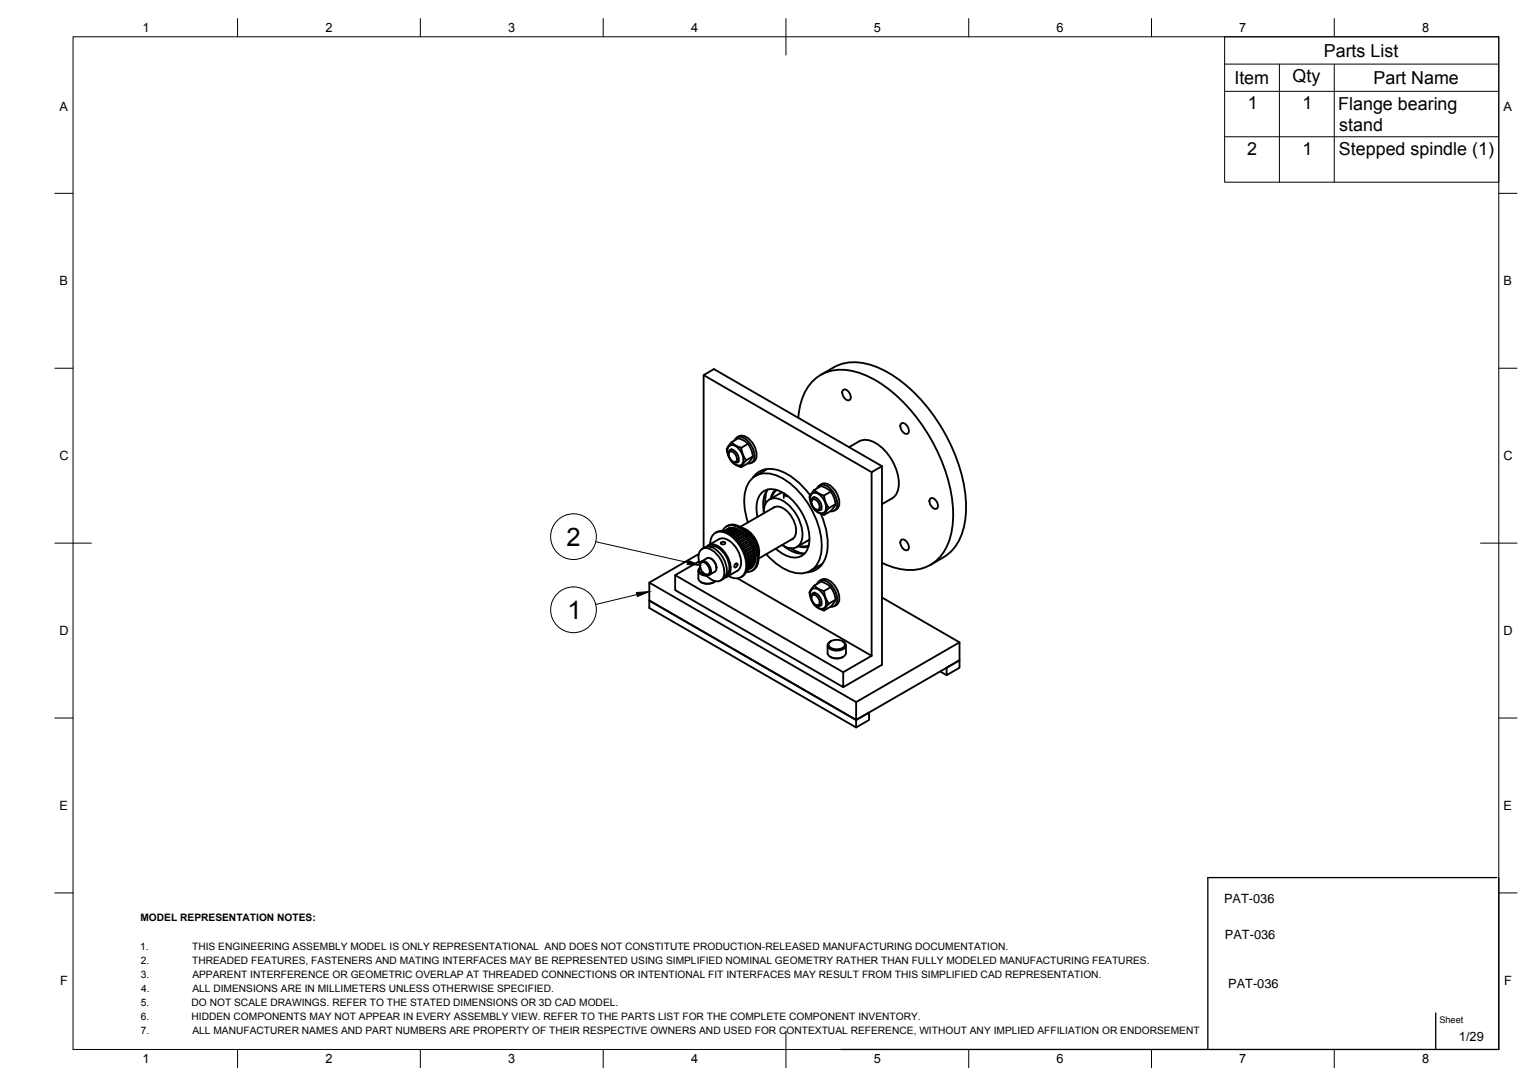
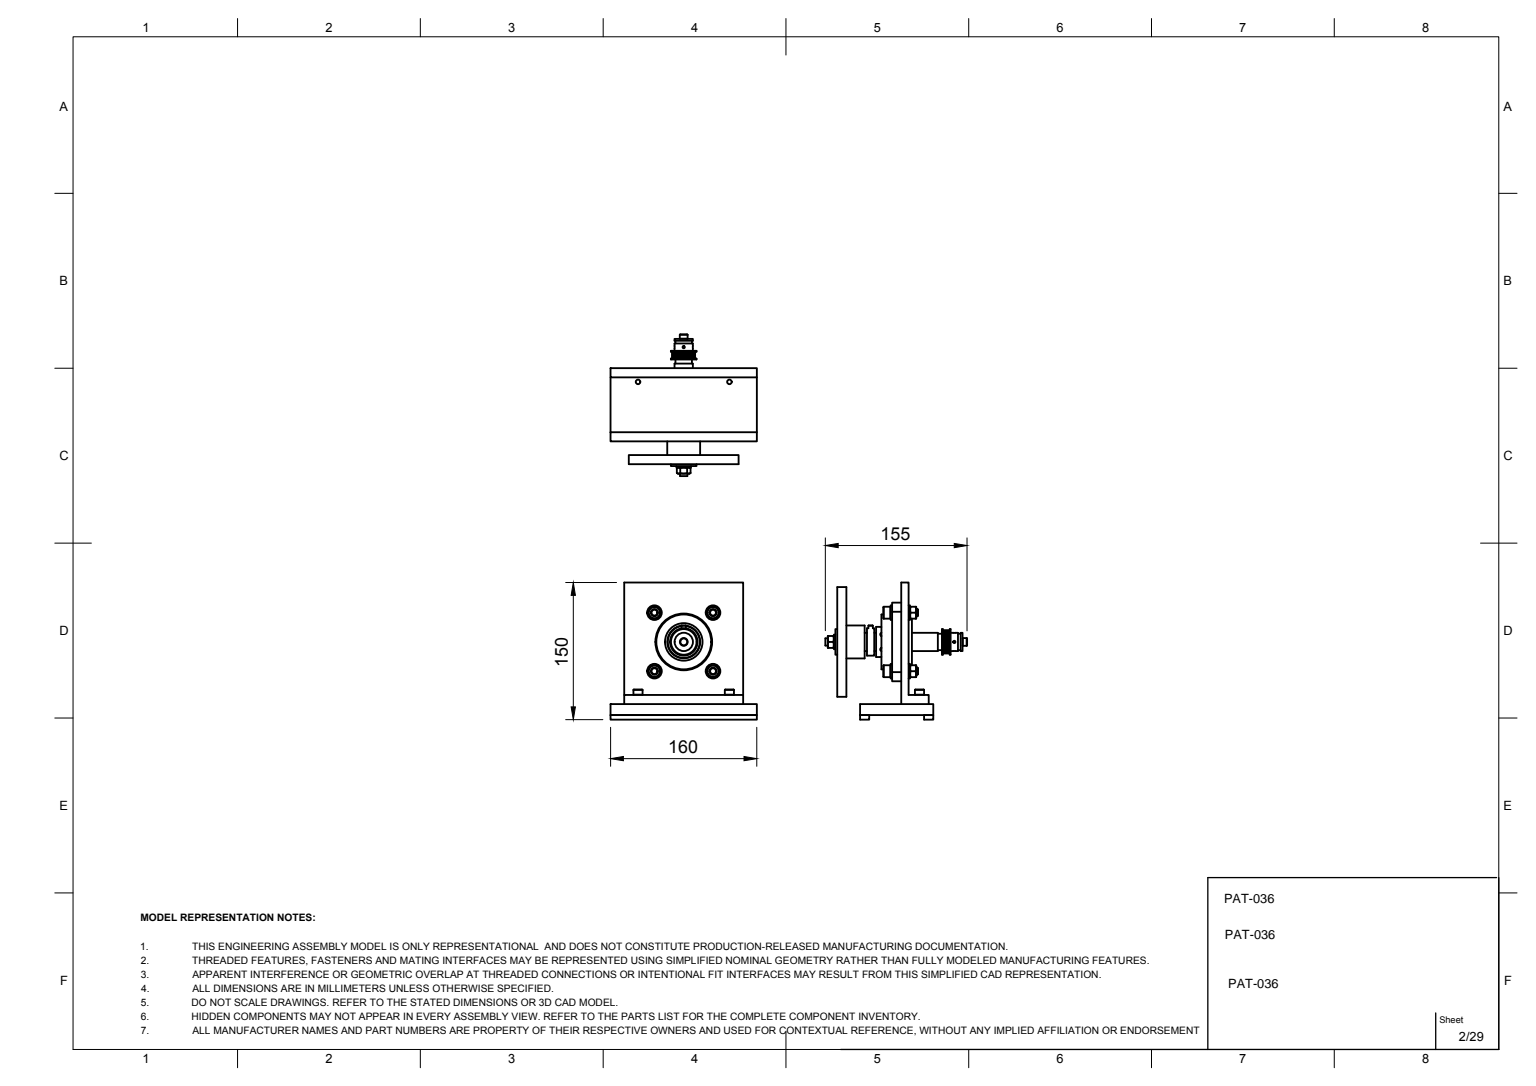
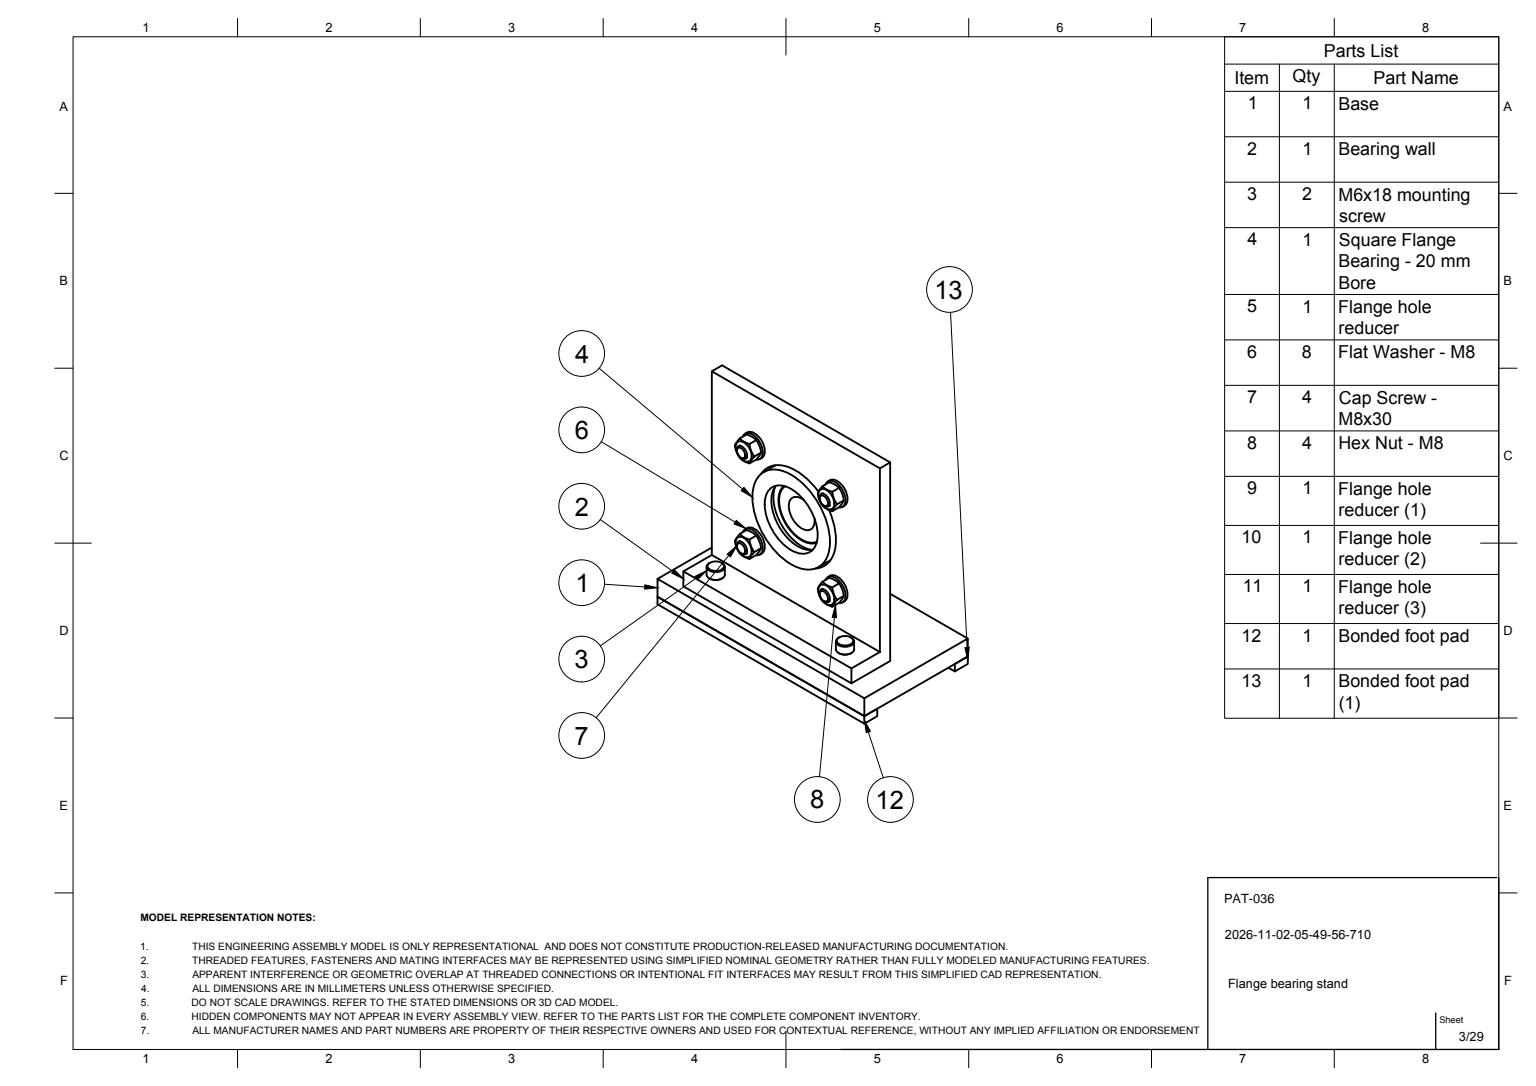
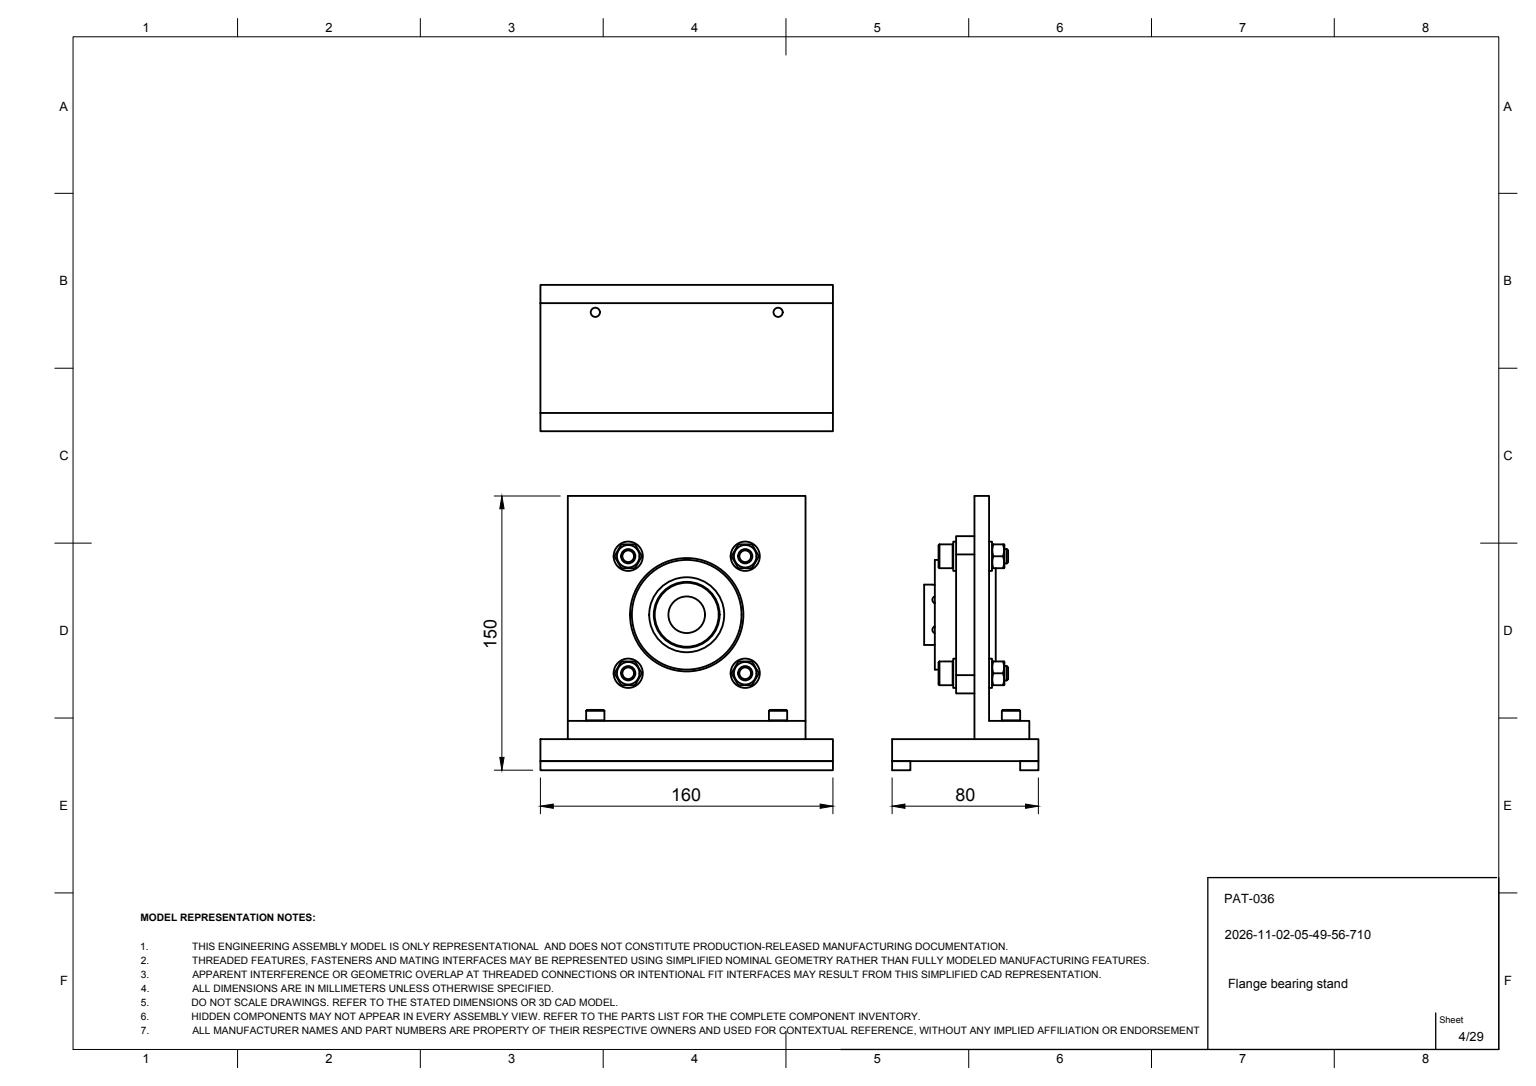
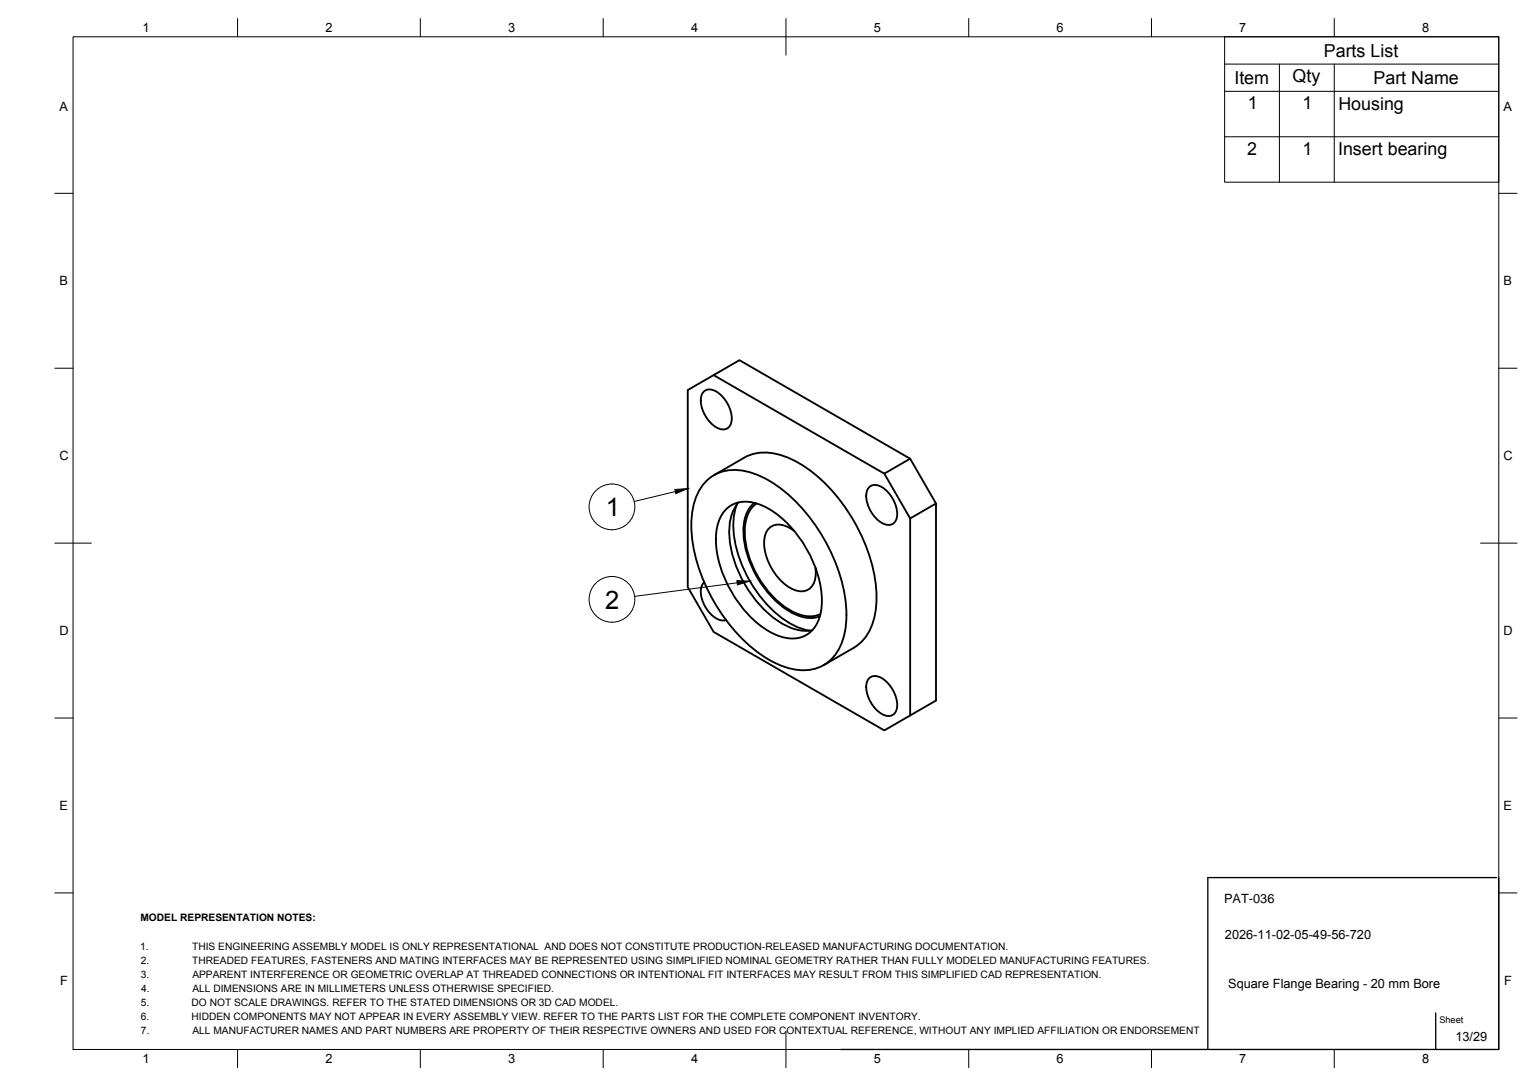
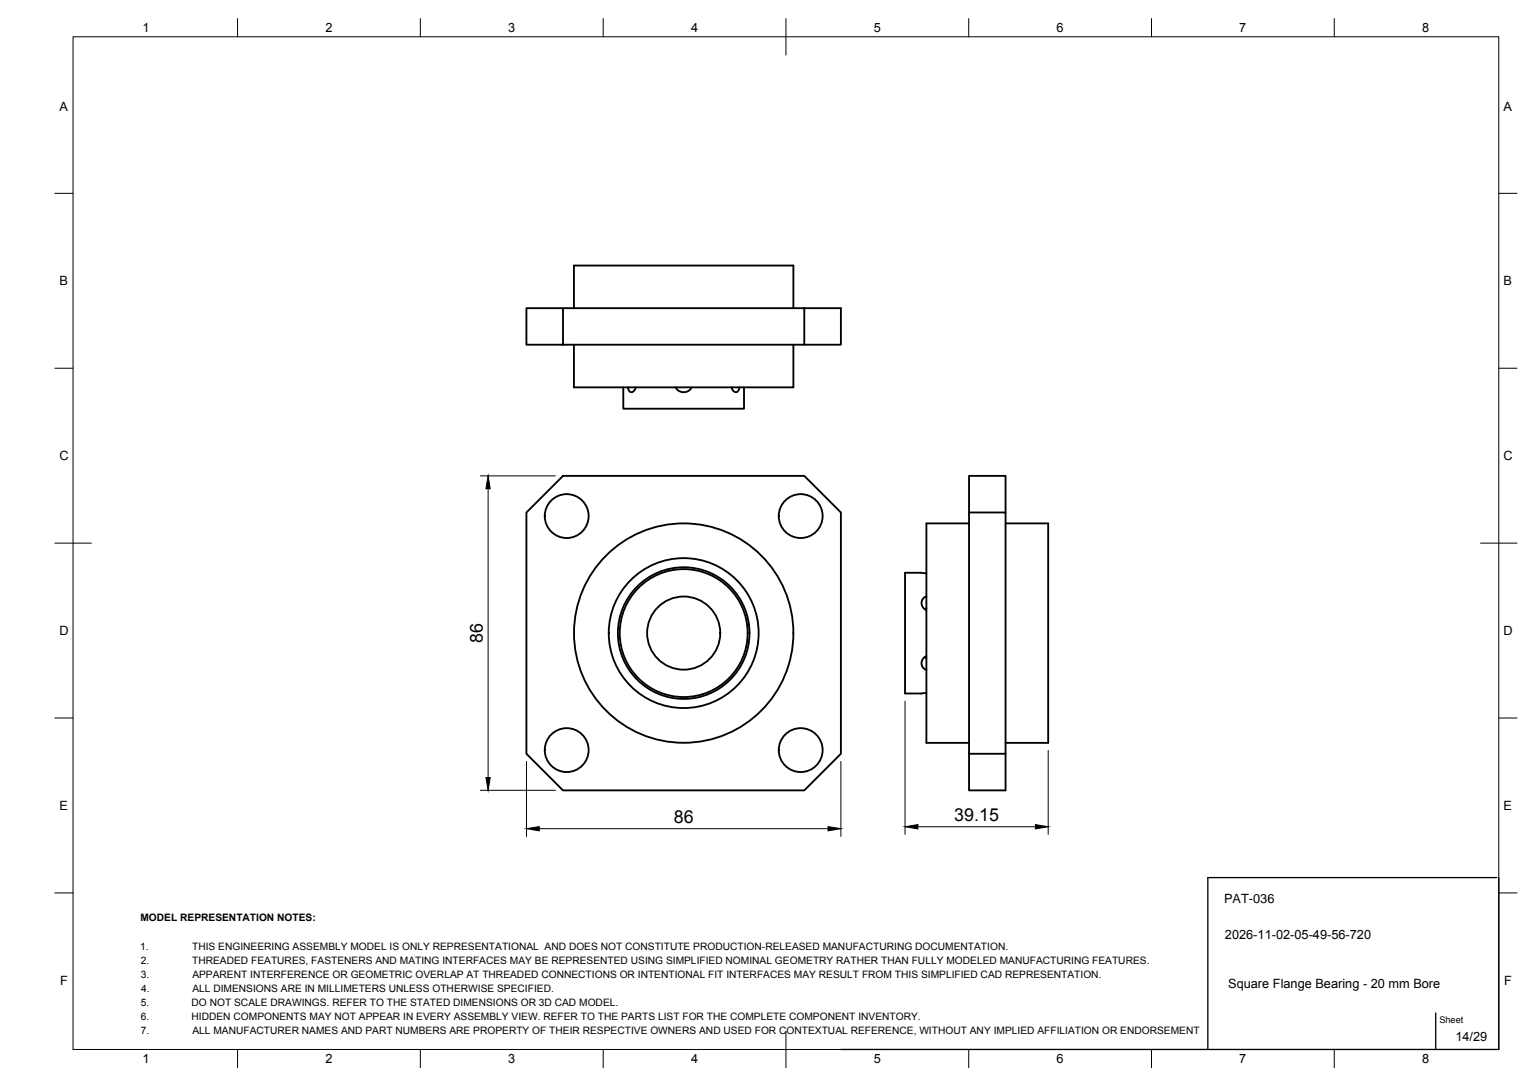
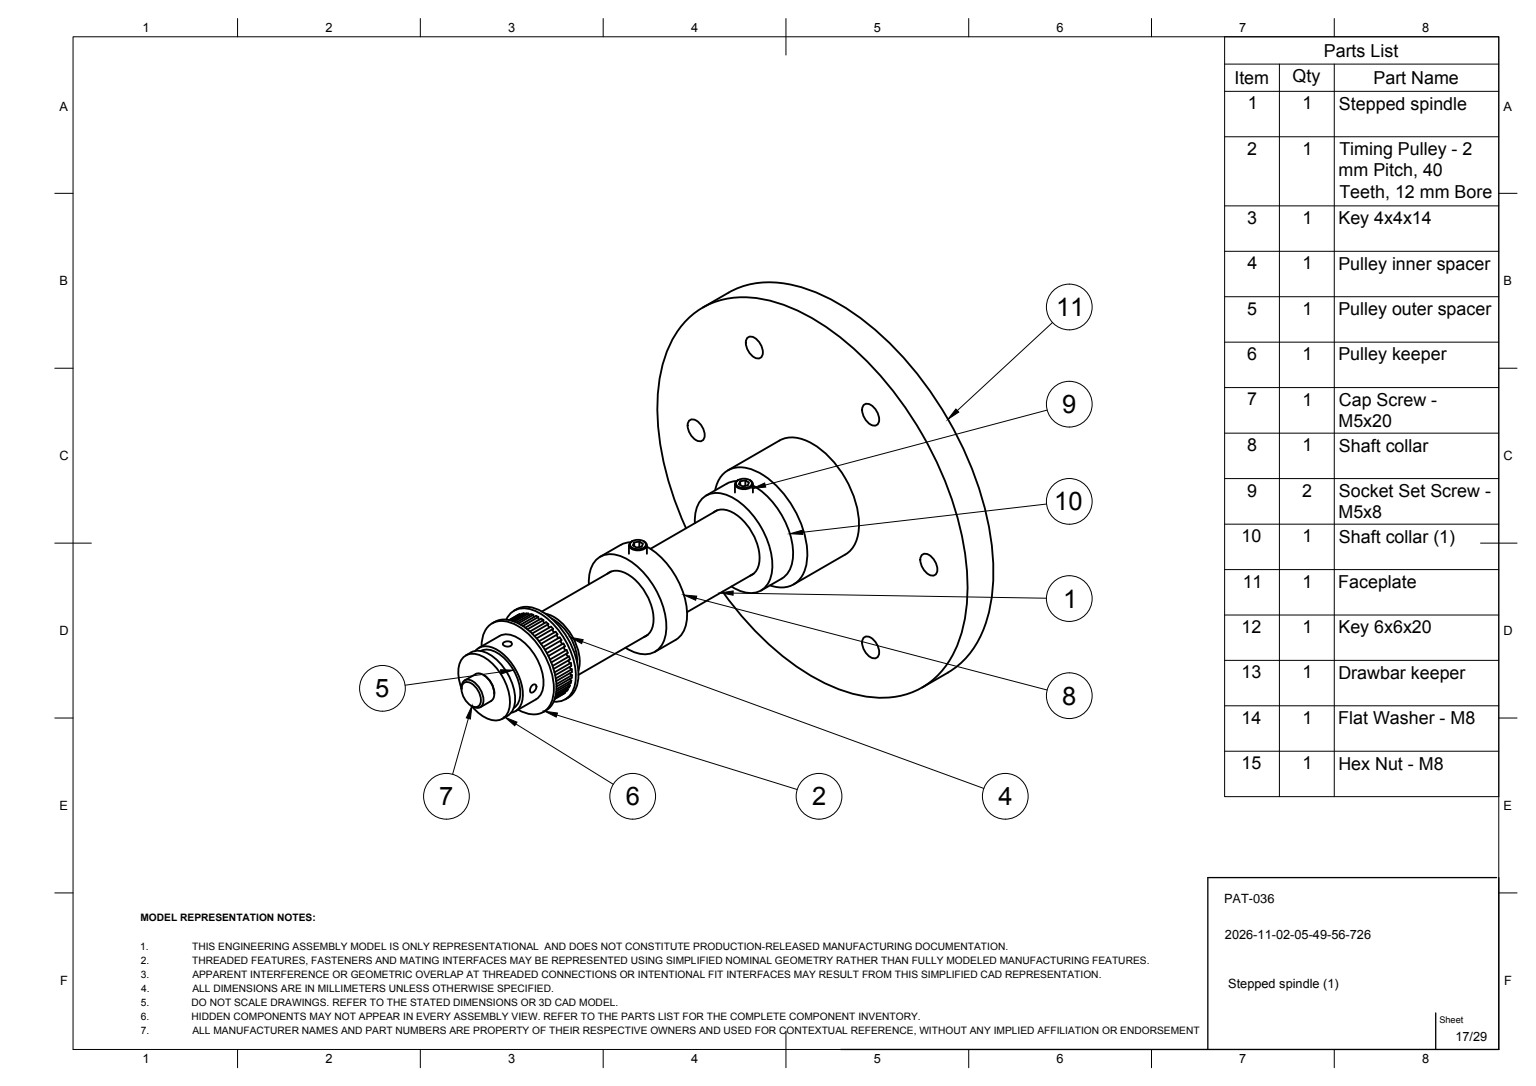
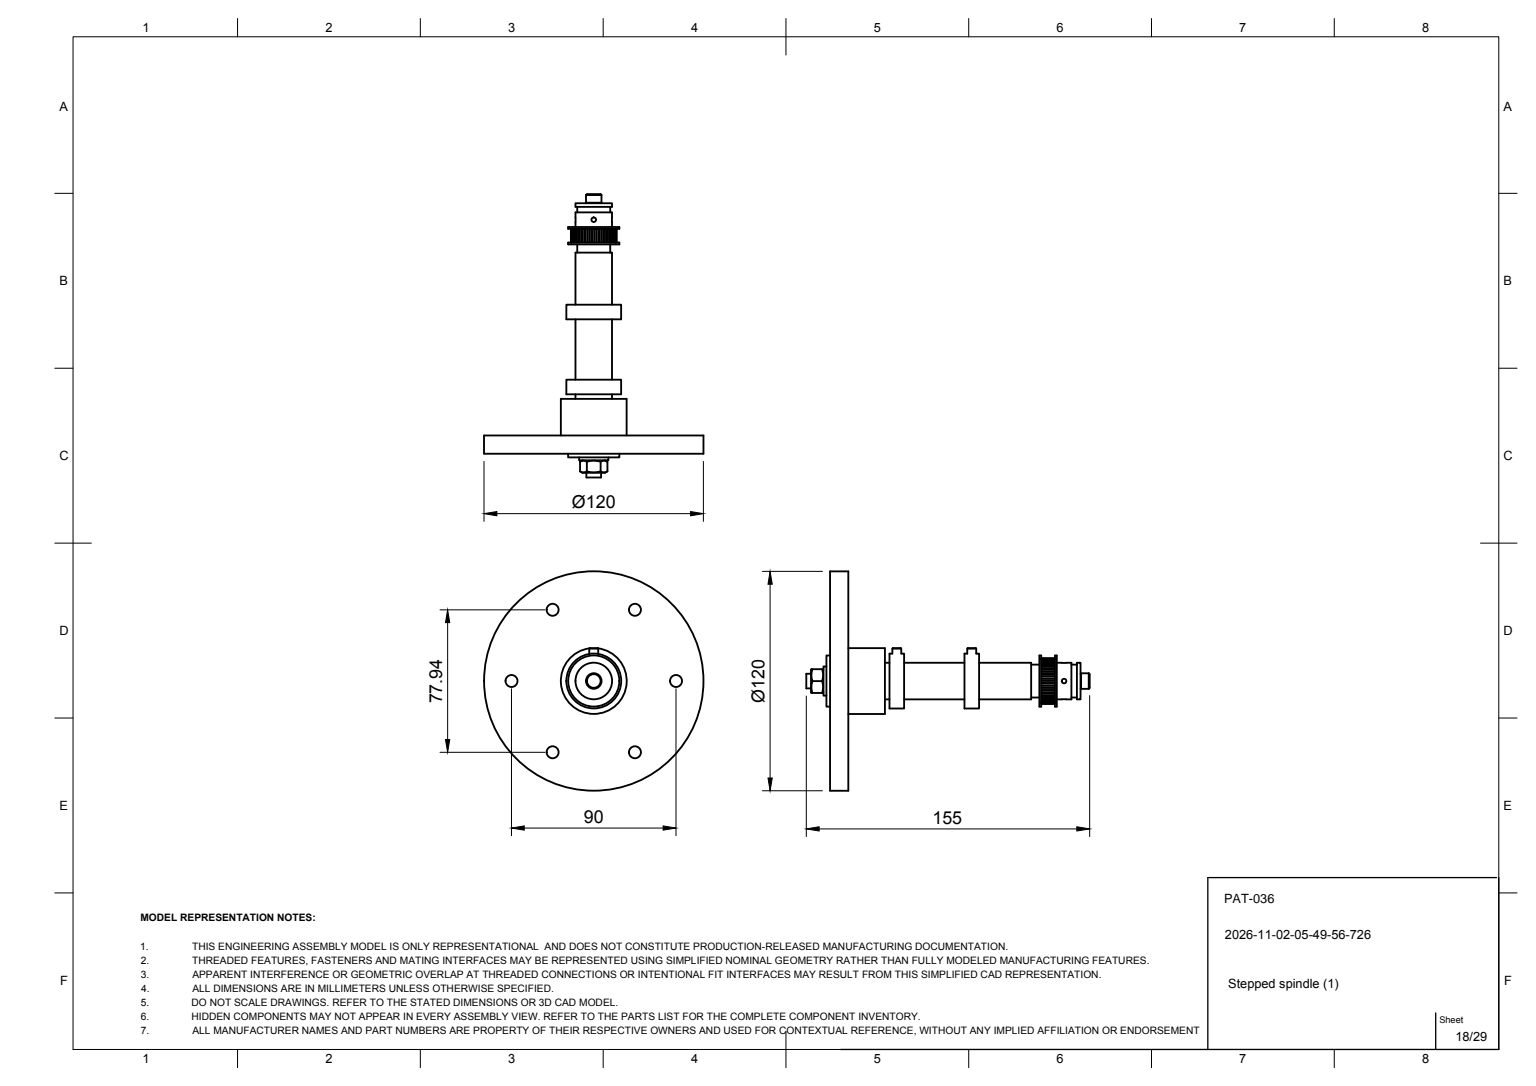
ISO-10303-21;
HEADER;
/* Generated by software containing ST-Developer
 * from STEP Tools, Inc. (www.steptools.com) 
 */

FILE_DESCRIPTION(
/* description */ ('Flange-mounted spindle'),
/* implementation_level */ '2;1');

FILE_NAME(
/* name */ 'PAT-036',
/* time_stamp */ '2026-10-27T10:49:51-07:00',
/* author */ (''),
/* organization */ (''),
/* preprocessor_version */ 'ST-DEVELOPER v20.2',
/* originating_system */ 'Autodesk Translation Framework v15.17.0.0',
/* authorisation */ '');

FILE_SCHEMA (('AUTOMOTIVE_DESIGN { 1 0 10303 214 3 1 1 }'));
ENDSEC;

DATA;
#10=MECHANICAL_DESIGN_GEOMETRIC_PRESENTATION_REPRESENTATION('',(#338,#339,
#340,#341,#342,#343,#344,#345,#346,#347,#348,#349,#350,#351,#352,#353,#354,
#355,#356,#357,#358,#359,#360,#361,#362,#363,#364,#365),#11764);
#11=(
BOUNDED_CURVE()
B_SPLINE_CURVE(2,(#11583,#11584,#11585),.UNSPECIFIED.,.F.,.F.)
B_SPLINE_CURVE_WITH_KNOTS((3,3),(0.14973948338295,0.97160236658079),
 .UNSPECIFIED.)
CURVE()
GEOMETRIC_REPRESENTATION_ITEM()
RATIONAL_B_SPLINE_CURVE((1.07140024848292,1.23714644374248,1.07140024848292))
REPRESENTATION_ITEM('')
);
#12=(
BOUNDED_CURVE()
B_SPLINE_CURVE(2,(#11587,#11588,#11589),.UNSPECIFIED.,.F.,.F.)
B_SPLINE_CURVE_WITH_KNOTS((3,3),(0.14973948338295,0.971602366580789),
 .UNSPECIFIED.)
CURVE()
GEOMETRIC_REPRESENTATION_ITEM()
RATIONAL_B_SPLINE_CURVE((1.07140024848292,1.23714644374248,1.07140024848292))
REPRESENTATION_ITEM('')
);
#13=(
BOUNDED_CURVE()
B_SPLINE_CURVE(2,(#11594,#11595,#11596),.UNSPECIFIED.,.F.,.F.)
B_SPLINE_CURVE_WITH_KNOTS((3,3),(0.14973948338295,0.97160236658079),
 .UNSPECIFIED.)
CURVE()
GEOMETRIC_REPRESENTATION_ITEM()
RATIONAL_B_SPLINE_CURVE((1.07140024848292,1.23714644374248,1.07140024848292))
REPRESENTATION_ITEM('')
);
#14=(
BOUNDED_CURVE()
B_SPLINE_CURVE(2,(#11598,#11599,#11600),.UNSPECIFIED.,.F.,.F.)
B_SPLINE_CURVE_WITH_KNOTS((3,3),(0.14973948338295,0.97160236658079),
 .UNSPECIFIED.)
CURVE()
GEOMETRIC_REPRESENTATION_ITEM()
RATIONAL_B_SPLINE_CURVE((1.07140024848292,1.23714644374248,1.07140024848292))
REPRESENTATION_ITEM('')
);
#15=(
BOUNDED_CURVE()
B_SPLINE_CURVE(2,(#11602,#11603,#11604),.UNSPECIFIED.,.F.,.F.)
B_SPLINE_CURVE_WITH_KNOTS((3,3),(0.14973948338295,0.971602366580789),
 .UNSPECIFIED.)
CURVE()
GEOMETRIC_REPRESENTATION_ITEM()
RATIONAL_B_SPLINE_CURVE((1.07140024848292,1.23714644374248,1.07140024848292))
REPRESENTATION_ITEM('')
);
#16=(
BOUNDED_CURVE()
B_SPLINE_CURVE(2,(#11605,#11606,#11607),.UNSPECIFIED.,.F.,.F.)
B_SPLINE_CURVE_WITH_KNOTS((3,3),(0.14973948338295,0.97160236658079),
 .UNSPECIFIED.)
CURVE()
GEOMETRIC_REPRESENTATION_ITEM()
RATIONAL_B_SPLINE_CURVE((1.07140024848292,1.23714644374248,1.07140024848292))
REPRESENTATION_ITEM('')
);
#17=(
BOUNDED_CURVE()
B_SPLINE_CURVE(2,(#11614,#11615,#11616),.UNSPECIFIED.,.F.,.F.)
B_SPLINE_CURVE_WITH_KNOTS((3,3),(0.14973948338295,0.97160236658079),
 .UNSPECIFIED.)
CURVE()
GEOMETRIC_REPRESENTATION_ITEM()
RATIONAL_B_SPLINE_CURVE((1.07140024848292,1.23714644374248,1.07140024848292))
REPRESENTATION_ITEM('')
);
#18=(
BOUNDED_CURVE()
B_SPLINE_CURVE(2,(#11618,#11619,#11620),.UNSPECIFIED.,.F.,.F.)
B_SPLINE_CURVE_WITH_KNOTS((3,3),(0.14973948338295,0.97160236658079),
 .UNSPECIFIED.)
CURVE()
GEOMETRIC_REPRESENTATION_ITEM()
RATIONAL_B_SPLINE_CURVE((1.07140024848292,1.23714644374248,1.07140024848292))
REPRESENTATION_ITEM('')
);
#19=(
BOUNDED_CURVE()
B_SPLINE_CURVE(2,(#11622,#11623,#11624),.UNSPECIFIED.,.F.,.F.)
B_SPLINE_CURVE_WITH_KNOTS((3,3),(0.14973948338295,0.971602366580789),
 .UNSPECIFIED.)
CURVE()
GEOMETRIC_REPRESENTATION_ITEM()
RATIONAL_B_SPLINE_CURVE((1.07140024848292,1.23714644374248,1.07140024848292))
REPRESENTATION_ITEM('')
);
#20=(
BOUNDED_CURVE()
B_SPLINE_CURVE(2,(#11626,#11627,#11628),.UNSPECIFIED.,.F.,.F.)
B_SPLINE_CURVE_WITH_KNOTS((3,3),(0.14973948338295,0.97160236658079),
 .UNSPECIFIED.)
CURVE()
GEOMETRIC_REPRESENTATION_ITEM()
RATIONAL_B_SPLINE_CURVE((1.07140024848292,1.23714644374248,1.07140024848292))
REPRESENTATION_ITEM('')
);
#21=(
BOUNDED_CURVE()
B_SPLINE_CURVE(2,(#11630,#11631,#11632),.UNSPECIFIED.,.F.,.F.)
B_SPLINE_CURVE_WITH_KNOTS((3,3),(0.14973948338295,0.97160236658079),
 .UNSPECIFIED.)
CURVE()
GEOMETRIC_REPRESENTATION_ITEM()
RATIONAL_B_SPLINE_CURVE((1.07140024848292,1.23714644374248,1.07140024848292))
REPRESENTATION_ITEM('')
);
#22=(
BOUNDED_CURVE()
B_SPLINE_CURVE(2,(#11633,#11634,#11635),.UNSPECIFIED.,.F.,.F.)
B_SPLINE_CURVE_WITH_KNOTS((3,3),(0.14973948338295,0.971602366580789),
 .UNSPECIFIED.)
CURVE()
GEOMETRIC_REPRESENTATION_ITEM()
RATIONAL_B_SPLINE_CURVE((1.07140024848292,1.23714644374248,1.07140024848292))
REPRESENTATION_ITEM('')
);
#23=ITEM_DEFINED_TRANSFORMATION($,$,#6579,#6646);
#24=ITEM_DEFINED_TRANSFORMATION($,$,#6618,#6647);
#25=ITEM_DEFINED_TRANSFORMATION($,$,#6461,#7163);
#26=ITEM_DEFINED_TRANSFORMATION($,$,#6474,#7164);
#27=ITEM_DEFINED_TRANSFORMATION($,$,#6504,#7165);
#28=ITEM_DEFINED_TRANSFORMATION($,$,#6513,#7166);
#29=ITEM_DEFINED_TRANSFORMATION($,$,#6522,#7167);
#30=ITEM_DEFINED_TRANSFORMATION($,$,#6531,#7168);
#31=ITEM_DEFINED_TRANSFORMATION($,$,#6540,#7169);
#32=ITEM_DEFINED_TRANSFORMATION($,$,#6547,#7170);
#33=ITEM_DEFINED_TRANSFORMATION($,$,#6554,#7171);
#34=ITEM_DEFINED_TRANSFORMATION($,$,#6554,#7172);
#35=ITEM_DEFINED_TRANSFORMATION($,$,#6578,#7173);
#36=ITEM_DEFINED_TRANSFORMATION($,$,#7138,#7174);
#37=ITEM_DEFINED_TRANSFORMATION($,$,#6648,#7175);
#38=ITEM_DEFINED_TRANSFORMATION($,$,#7138,#7176);
#39=ITEM_DEFINED_TRANSFORMATION($,$,#7147,#7177);
#40=ITEM_DEFINED_TRANSFORMATION($,$,#7138,#7178);
#41=ITEM_DEFINED_TRANSFORMATION($,$,#6648,#7179);
#42=ITEM_DEFINED_TRANSFORMATION($,$,#7138,#7180);
#43=ITEM_DEFINED_TRANSFORMATION($,$,#7147,#7181);
#44=ITEM_DEFINED_TRANSFORMATION($,$,#7138,#7182);
#45=ITEM_DEFINED_TRANSFORMATION($,$,#6648,#7183);
#46=ITEM_DEFINED_TRANSFORMATION($,$,#7138,#7184);
#47=ITEM_DEFINED_TRANSFORMATION($,$,#7147,#7185);
#48=ITEM_DEFINED_TRANSFORMATION($,$,#7138,#7186);
#49=ITEM_DEFINED_TRANSFORMATION($,$,#6648,#7187);
#50=ITEM_DEFINED_TRANSFORMATION($,$,#7138,#7188);
#51=ITEM_DEFINED_TRANSFORMATION($,$,#7147,#7189);
#52=ITEM_DEFINED_TRANSFORMATION($,$,#6675,#7190);
#53=ITEM_DEFINED_TRANSFORMATION($,$,#6707,#7191);
#54=ITEM_DEFINED_TRANSFORMATION($,$,#6716,#7192);
#55=ITEM_DEFINED_TRANSFORMATION($,$,#6725,#7193);
#56=ITEM_DEFINED_TRANSFORMATION($,$,#6734,#7194);
#57=ITEM_DEFINED_TRANSFORMATION($,$,#6749,#7195);
#58=ITEM_DEFINED_TRANSFORMATION($,$,#6764,#7196);
#59=ITEM_DEFINED_TRANSFORMATION($,$,#6798,#7197);
#60=ITEM_DEFINED_TRANSFORMATION($,$,#6807,#7198);
#61=ITEM_DEFINED_TRANSFORMATION($,$,#7073,#7199);
#62=ITEM_DEFINED_TRANSFORMATION($,$,#7084,#7200);
#63=ITEM_DEFINED_TRANSFORMATION($,$,#7110,#7201);
#64=ITEM_DEFINED_TRANSFORMATION($,$,#7110,#7202);
#65=ITEM_DEFINED_TRANSFORMATION($,$,#7127,#7203);
#66=ITEM_DEFINED_TRANSFORMATION($,$,#7138,#7204);
#67=ITEM_DEFINED_TRANSFORMATION($,$,#7147,#7205);
#68=ITEM_DEFINED_TRANSFORMATION($,$,#6460,#7206);
#69=ITEM_DEFINED_TRANSFORMATION($,$,#6674,#7207);
#70=(
REPRESENTATION_RELATIONSHIP($,$,#11890,#11889)
REPRESENTATION_RELATIONSHIP_WITH_TRANSFORMATION(#23)
SHAPE_REPRESENTATION_RELATIONSHIP()
);
#71=(
REPRESENTATION_RELATIONSHIP($,$,#11891,#11889)
REPRESENTATION_RELATIONSHIP_WITH_TRANSFORMATION(#24)
SHAPE_REPRESENTATION_RELATIONSHIP()
);
#72=(
REPRESENTATION_RELATIONSHIP($,$,#11880,#11879)
REPRESENTATION_RELATIONSHIP_WITH_TRANSFORMATION(#25)
SHAPE_REPRESENTATION_RELATIONSHIP()
);
#73=(
REPRESENTATION_RELATIONSHIP($,$,#11881,#11879)
REPRESENTATION_RELATIONSHIP_WITH_TRANSFORMATION(#26)
SHAPE_REPRESENTATION_RELATIONSHIP()
);
#74=(
REPRESENTATION_RELATIONSHIP($,$,#11882,#11879)
REPRESENTATION_RELATIONSHIP_WITH_TRANSFORMATION(#27)
SHAPE_REPRESENTATION_RELATIONSHIP()
);
#75=(
REPRESENTATION_RELATIONSHIP($,$,#11883,#11879)
REPRESENTATION_RELATIONSHIP_WITH_TRANSFORMATION(#28)
SHAPE_REPRESENTATION_RELATIONSHIP()
);
#76=(
REPRESENTATION_RELATIONSHIP($,$,#11884,#11879)
REPRESENTATION_RELATIONSHIP_WITH_TRANSFORMATION(#29)
SHAPE_REPRESENTATION_RELATIONSHIP()
);
#77=(
REPRESENTATION_RELATIONSHIP($,$,#11885,#11879)
REPRESENTATION_RELATIONSHIP_WITH_TRANSFORMATION(#30)
SHAPE_REPRESENTATION_RELATIONSHIP()
);
#78=(
REPRESENTATION_RELATIONSHIP($,$,#11886,#11879)
REPRESENTATION_RELATIONSHIP_WITH_TRANSFORMATION(#31)
SHAPE_REPRESENTATION_RELATIONSHIP()
);
#79=(
REPRESENTATION_RELATIONSHIP($,$,#11887,#11879)
REPRESENTATION_RELATIONSHIP_WITH_TRANSFORMATION(#32)
SHAPE_REPRESENTATION_RELATIONSHIP()
);
#80=(
REPRESENTATION_RELATIONSHIP($,$,#11888,#11879)
REPRESENTATION_RELATIONSHIP_WITH_TRANSFORMATION(#33)
SHAPE_REPRESENTATION_RELATIONSHIP()
);
#81=(
REPRESENTATION_RELATIONSHIP($,$,#11888,#11879)
REPRESENTATION_RELATIONSHIP_WITH_TRANSFORMATION(#34)
SHAPE_REPRESENTATION_RELATIONSHIP()
);
#82=(
REPRESENTATION_RELATIONSHIP($,$,#11889,#11879)
REPRESENTATION_RELATIONSHIP_WITH_TRANSFORMATION(#35)
SHAPE_REPRESENTATION_RELATIONSHIP()
);
#83=(
REPRESENTATION_RELATIONSHIP($,$,#11907,#11879)
REPRESENTATION_RELATIONSHIP_WITH_TRANSFORMATION(#36)
SHAPE_REPRESENTATION_RELATIONSHIP()
);
#84=(
REPRESENTATION_RELATIONSHIP($,$,#11892,#11879)
REPRESENTATION_RELATIONSHIP_WITH_TRANSFORMATION(#37)
SHAPE_REPRESENTATION_RELATIONSHIP()
);
#85=(
REPRESENTATION_RELATIONSHIP($,$,#11907,#11879)
REPRESENTATION_RELATIONSHIP_WITH_TRANSFORMATION(#38)
SHAPE_REPRESENTATION_RELATIONSHIP()
);
#86=(
REPRESENTATION_RELATIONSHIP($,$,#11908,#11879)
REPRESENTATION_RELATIONSHIP_WITH_TRANSFORMATION(#39)
SHAPE_REPRESENTATION_RELATIONSHIP()
);
#87=(
REPRESENTATION_RELATIONSHIP($,$,#11907,#11879)
REPRESENTATION_RELATIONSHIP_WITH_TRANSFORMATION(#40)
SHAPE_REPRESENTATION_RELATIONSHIP()
);
#88=(
REPRESENTATION_RELATIONSHIP($,$,#11892,#11879)
REPRESENTATION_RELATIONSHIP_WITH_TRANSFORMATION(#41)
SHAPE_REPRESENTATION_RELATIONSHIP()
);
#89=(
REPRESENTATION_RELATIONSHIP($,$,#11907,#11879)
REPRESENTATION_RELATIONSHIP_WITH_TRANSFORMATION(#42)
SHAPE_REPRESENTATION_RELATIONSHIP()
);
#90=(
REPRESENTATION_RELATIONSHIP($,$,#11908,#11879)
REPRESENTATION_RELATIONSHIP_WITH_TRANSFORMATION(#43)
SHAPE_REPRESENTATION_RELATIONSHIP()
);
#91=(
REPRESENTATION_RELATIONSHIP($,$,#11907,#11879)
REPRESENTATION_RELATIONSHIP_WITH_TRANSFORMATION(#44)
SHAPE_REPRESENTATION_RELATIONSHIP()
);
#92=(
REPRESENTATION_RELATIONSHIP($,$,#11892,#11879)
REPRESENTATION_RELATIONSHIP_WITH_TRANSFORMATION(#45)
SHAPE_REPRESENTATION_RELATIONSHIP()
);
#93=(
REPRESENTATION_RELATIONSHIP($,$,#11907,#11879)
REPRESENTATION_RELATIONSHIP_WITH_TRANSFORMATION(#46)
SHAPE_REPRESENTATION_RELATIONSHIP()
);
#94=(
REPRESENTATION_RELATIONSHIP($,$,#11908,#11879)
REPRESENTATION_RELATIONSHIP_WITH_TRANSFORMATION(#47)
SHAPE_REPRESENTATION_RELATIONSHIP()
);
#95=(
REPRESENTATION_RELATIONSHIP($,$,#11907,#11879)
REPRESENTATION_RELATIONSHIP_WITH_TRANSFORMATION(#48)
SHAPE_REPRESENTATION_RELATIONSHIP()
);
#96=(
REPRESENTATION_RELATIONSHIP($,$,#11892,#11879)
REPRESENTATION_RELATIONSHIP_WITH_TRANSFORMATION(#49)
SHAPE_REPRESENTATION_RELATIONSHIP()
);
#97=(
REPRESENTATION_RELATIONSHIP($,$,#11907,#11879)
REPRESENTATION_RELATIONSHIP_WITH_TRANSFORMATION(#50)
SHAPE_REPRESENTATION_RELATIONSHIP()
);
#98=(
REPRESENTATION_RELATIONSHIP($,$,#11908,#11879)
REPRESENTATION_RELATIONSHIP_WITH_TRANSFORMATION(#51)
SHAPE_REPRESENTATION_RELATIONSHIP()
);
#99=(
REPRESENTATION_RELATIONSHIP($,$,#11894,#11893)
REPRESENTATION_RELATIONSHIP_WITH_TRANSFORMATION(#52)
SHAPE_REPRESENTATION_RELATIONSHIP()
);
#100=(
REPRESENTATION_RELATIONSHIP($,$,#11895,#11893)
REPRESENTATION_RELATIONSHIP_WITH_TRANSFORMATION(#53)
SHAPE_REPRESENTATION_RELATIONSHIP()
);
#101=(
REPRESENTATION_RELATIONSHIP($,$,#11896,#11893)
REPRESENTATION_RELATIONSHIP_WITH_TRANSFORMATION(#54)
SHAPE_REPRESENTATION_RELATIONSHIP()
);
#102=(
REPRESENTATION_RELATIONSHIP($,$,#11897,#11893)
REPRESENTATION_RELATIONSHIP_WITH_TRANSFORMATION(#55)
SHAPE_REPRESENTATION_RELATIONSHIP()
);
#103=(
REPRESENTATION_RELATIONSHIP($,$,#11898,#11893)
REPRESENTATION_RELATIONSHIP_WITH_TRANSFORMATION(#56)
SHAPE_REPRESENTATION_RELATIONSHIP()
);
#104=(
REPRESENTATION_RELATIONSHIP($,$,#11899,#11893)
REPRESENTATION_RELATIONSHIP_WITH_TRANSFORMATION(#57)
SHAPE_REPRESENTATION_RELATIONSHIP()
);
#105=(
REPRESENTATION_RELATIONSHIP($,$,#11900,#11893)
REPRESENTATION_RELATIONSHIP_WITH_TRANSFORMATION(#58)
SHAPE_REPRESENTATION_RELATIONSHIP()
);
#106=(
REPRESENTATION_RELATIONSHIP($,$,#11901,#11893)
REPRESENTATION_RELATIONSHIP_WITH_TRANSFORMATION(#59)
SHAPE_REPRESENTATION_RELATIONSHIP()
);
#107=(
REPRESENTATION_RELATIONSHIP($,$,#11902,#11893)
REPRESENTATION_RELATIONSHIP_WITH_TRANSFORMATION(#60)
SHAPE_REPRESENTATION_RELATIONSHIP()
);
#108=(
REPRESENTATION_RELATIONSHIP($,$,#11903,#11893)
REPRESENTATION_RELATIONSHIP_WITH_TRANSFORMATION(#61)
SHAPE_REPRESENTATION_RELATIONSHIP()
);
#109=(
REPRESENTATION_RELATIONSHIP($,$,#11904,#11893)
REPRESENTATION_RELATIONSHIP_WITH_TRANSFORMATION(#62)
SHAPE_REPRESENTATION_RELATIONSHIP()
);
#110=(
REPRESENTATION_RELATIONSHIP($,$,#11905,#11893)
REPRESENTATION_RELATIONSHIP_WITH_TRANSFORMATION(#63)
SHAPE_REPRESENTATION_RELATIONSHIP()
);
#111=(
REPRESENTATION_RELATIONSHIP($,$,#11905,#11893)
REPRESENTATION_RELATIONSHIP_WITH_TRANSFORMATION(#64)
SHAPE_REPRESENTATION_RELATIONSHIP()
);
#112=(
REPRESENTATION_RELATIONSHIP($,$,#11906,#11893)
REPRESENTATION_RELATIONSHIP_WITH_TRANSFORMATION(#65)
SHAPE_REPRESENTATION_RELATIONSHIP()
);
#113=(
REPRESENTATION_RELATIONSHIP($,$,#11907,#11893)
REPRESENTATION_RELATIONSHIP_WITH_TRANSFORMATION(#66)
SHAPE_REPRESENTATION_RELATIONSHIP()
);
#114=(
REPRESENTATION_RELATIONSHIP($,$,#11908,#11893)
REPRESENTATION_RELATIONSHIP_WITH_TRANSFORMATION(#67)
SHAPE_REPRESENTATION_RELATIONSHIP()
);
#115=(
REPRESENTATION_RELATIONSHIP($,$,#11879,#11878)
REPRESENTATION_RELATIONSHIP_WITH_TRANSFORMATION(#68)
SHAPE_REPRESENTATION_RELATIONSHIP()
);
#116=(
REPRESENTATION_RELATIONSHIP($,$,#11893,#11878)
REPRESENTATION_RELATIONSHIP_WITH_TRANSFORMATION(#69)
SHAPE_REPRESENTATION_RELATIONSHIP()
);
#117=CONTEXT_DEPENDENT_SHAPE_REPRESENTATION(#70,#11814);
#118=CONTEXT_DEPENDENT_SHAPE_REPRESENTATION(#71,#11815);
#119=CONTEXT_DEPENDENT_SHAPE_REPRESENTATION(#72,#11833);
#120=CONTEXT_DEPENDENT_SHAPE_REPRESENTATION(#73,#11834);
#121=CONTEXT_DEPENDENT_SHAPE_REPRESENTATION(#74,#11835);
#122=CONTEXT_DEPENDENT_SHAPE_REPRESENTATION(#75,#11836);
#123=CONTEXT_DEPENDENT_SHAPE_REPRESENTATION(#76,#11837);
#124=CONTEXT_DEPENDENT_SHAPE_REPRESENTATION(#77,#11838);
#125=CONTEXT_DEPENDENT_SHAPE_REPRESENTATION(#78,#11839);
#126=CONTEXT_DEPENDENT_SHAPE_REPRESENTATION(#79,#11840);
#127=CONTEXT_DEPENDENT_SHAPE_REPRESENTATION(#80,#11841);
#128=CONTEXT_DEPENDENT_SHAPE_REPRESENTATION(#81,#11842);
#129=CONTEXT_DEPENDENT_SHAPE_REPRESENTATION(#82,#11843);
#130=CONTEXT_DEPENDENT_SHAPE_REPRESENTATION(#83,#11844);
#131=CONTEXT_DEPENDENT_SHAPE_REPRESENTATION(#84,#11845);
#132=CONTEXT_DEPENDENT_SHAPE_REPRESENTATION(#85,#11846);
#133=CONTEXT_DEPENDENT_SHAPE_REPRESENTATION(#86,#11847);
#134=CONTEXT_DEPENDENT_SHAPE_REPRESENTATION(#87,#11848);
#135=CONTEXT_DEPENDENT_SHAPE_REPRESENTATION(#88,#11849);
#136=CONTEXT_DEPENDENT_SHAPE_REPRESENTATION(#89,#11850);
#137=CONTEXT_DEPENDENT_SHAPE_REPRESENTATION(#90,#11851);
#138=CONTEXT_DEPENDENT_SHAPE_REPRESENTATION(#91,#11852);
#139=CONTEXT_DEPENDENT_SHAPE_REPRESENTATION(#92,#11853);
#140=CONTEXT_DEPENDENT_SHAPE_REPRESENTATION(#93,#11854);
#141=CONTEXT_DEPENDENT_SHAPE_REPRESENTATION(#94,#11855);
#142=CONTEXT_DEPENDENT_SHAPE_REPRESENTATION(#95,#11856);
#143=CONTEXT_DEPENDENT_SHAPE_REPRESENTATION(#96,#11857);
#144=CONTEXT_DEPENDENT_SHAPE_REPRESENTATION(#97,#11858);
#145=CONTEXT_DEPENDENT_SHAPE_REPRESENTATION(#98,#11859);
#146=CONTEXT_DEPENDENT_SHAPE_REPRESENTATION(#99,#11860);
#147=CONTEXT_DEPENDENT_SHAPE_REPRESENTATION(#100,#11861);
#148=CONTEXT_DEPENDENT_SHAPE_REPRESENTATION(#101,#11862);
#149=CONTEXT_DEPENDENT_SHAPE_REPRESENTATION(#102,#11863);
#150=CONTEXT_DEPENDENT_SHAPE_REPRESENTATION(#103,#11864);
#151=CONTEXT_DEPENDENT_SHAPE_REPRESENTATION(#104,#11865);
#152=CONTEXT_DEPENDENT_SHAPE_REPRESENTATION(#105,#11866);
#153=CONTEXT_DEPENDENT_SHAPE_REPRESENTATION(#106,#11867);
#154=CONTEXT_DEPENDENT_SHAPE_REPRESENTATION(#107,#11868);
#155=CONTEXT_DEPENDENT_SHAPE_REPRESENTATION(#108,#11869);
#156=CONTEXT_DEPENDENT_SHAPE_REPRESENTATION(#109,#11870);
#157=CONTEXT_DEPENDENT_SHAPE_REPRESENTATION(#110,#11871);
#158=CONTEXT_DEPENDENT_SHAPE_REPRESENTATION(#111,#11872);
#159=CONTEXT_DEPENDENT_SHAPE_REPRESENTATION(#112,#11873);
#160=CONTEXT_DEPENDENT_SHAPE_REPRESENTATION(#113,#11874);
#161=CONTEXT_DEPENDENT_SHAPE_REPRESENTATION(#114,#11875);
#162=CONTEXT_DEPENDENT_SHAPE_REPRESENTATION(#115,#11876);
#163=CONTEXT_DEPENDENT_SHAPE_REPRESENTATION(#116,#11877);
#164=NEXT_ASSEMBLY_USAGE_OCCURRENCE('Housing:1','Housing:1','Housing:1',
#11921,#11922,'Housing:1');
#165=NEXT_ASSEMBLY_USAGE_OCCURRENCE('Insert bearing:1',
'Insert bearing:1','Insert bearing:1',#11921,#11923,'Insert bearing:1');
#166=NEXT_ASSEMBLY_USAGE_OCCURRENCE('Base:1','Base:1','Base:1',#11911,#11912,
'Base:1');
#167=NEXT_ASSEMBLY_USAGE_OCCURRENCE('Bearing wall:1','Bearing wall:1',
'Bearing wall:1',#11911,#11913,'Bearing wall:1');
#168=NEXT_ASSEMBLY_USAGE_OCCURRENCE('Flange hole reducer:1',
'Flange hole reducer:1','Flange hole reducer:1',#11911,#11914,
'Flange hole reducer:1');
#169=NEXT_ASSEMBLY_USAGE_OCCURRENCE('Flange hole reducer (1):1',
'Flange hole reducer (1):1','Flange hole reducer (1):1',#11911,#11915,
'Flange hole reducer (1):1');
#170=NEXT_ASSEMBLY_USAGE_OCCURRENCE('Flange hole reducer (2):1',
'Flange hole reducer (2):1','Flange hole reducer (2):1',#11911,#11916,
'Flange hole reducer (2):1');
#171=NEXT_ASSEMBLY_USAGE_OCCURRENCE('Flange hole reducer (3):1',
'Flange hole reducer (3):1','Flange hole reducer (3):1',#11911,#11917,
'Flange hole reducer (3):1');
#172=NEXT_ASSEMBLY_USAGE_OCCURRENCE('Bonded foot pad:1',
'Bonded foot pad:1','Bonded foot pad:1',#11911,#11918,
'Bonded foot pad:1');
#173=NEXT_ASSEMBLY_USAGE_OCCURRENCE('Bonded foot pad (1):1',
'Bonded foot pad (1):1','Bonded foot pad (1):1',#11911,#11919,
'Bonded foot pad (1):1');
#174=NEXT_ASSEMBLY_USAGE_OCCURRENCE('M6x18 mounting screw:2',
'M6x18 mounting screw:2','M6x18 mounting screw:2',#11911,#11920,
'M6x18 mounting screw:2');
#175=NEXT_ASSEMBLY_USAGE_OCCURRENCE('M6x18 mounting screw:3',
'M6x18 mounting screw:3','M6x18 mounting screw:3',#11911,#11920,
'M6x18 mounting screw:3');
#176=NEXT_ASSEMBLY_USAGE_OCCURRENCE(
'Square Flange Bearing - 20 mm Bore:2',
'Square Flange Bearing - 20 mm Bore:2',
'Square Flange Bearing - 20 mm Bore:2',#11911,#11921,
'Square Flange Bearing - 20 mm Bore:2');
#177=NEXT_ASSEMBLY_USAGE_OCCURRENCE('Flat Washer - M8:2',
'Flat Washer - M8:2','Flat Washer - M8:2',#11911,#11939,
'Flat Washer - M8:2');
#178=NEXT_ASSEMBLY_USAGE_OCCURRENCE('Cap Screw - M8x30:2',
'Cap Screw - M8x30:2','Cap Screw - M8x30:2',#11911,#11924,
'Cap Screw - M8x30:2');
#179=NEXT_ASSEMBLY_USAGE_OCCURRENCE('Flat Washer - M8:3',
'Flat Washer - M8:3','Flat Washer - M8:3',#11911,#11939,
'Flat Washer - M8:3');
#180=NEXT_ASSEMBLY_USAGE_OCCURRENCE('Hex Nut - M8:2','Hex Nut - M8:2',
'Hex Nut - M8:2',#11911,#11940,'Hex Nut - M8:2');
#181=NEXT_ASSEMBLY_USAGE_OCCURRENCE('Flat Washer - M8:4',
'Flat Washer - M8:4','Flat Washer - M8:4',#11911,#11939,
'Flat Washer - M8:4');
#182=NEXT_ASSEMBLY_USAGE_OCCURRENCE('Cap Screw - M8x30:3',
'Cap Screw - M8x30:3','Cap Screw - M8x30:3',#11911,#11924,
'Cap Screw - M8x30:3');
#183=NEXT_ASSEMBLY_USAGE_OCCURRENCE('Flat Washer - M8:5',
'Flat Washer - M8:5','Flat Washer - M8:5',#11911,#11939,
'Flat Washer - M8:5');
#184=NEXT_ASSEMBLY_USAGE_OCCURRENCE('Hex Nut - M8:3','Hex Nut - M8:3',
'Hex Nut - M8:3',#11911,#11940,'Hex Nut - M8:3');
#185=NEXT_ASSEMBLY_USAGE_OCCURRENCE('Flat Washer - M8:6',
'Flat Washer - M8:6','Flat Washer - M8:6',#11911,#11939,
'Flat Washer - M8:6');
#186=NEXT_ASSEMBLY_USAGE_OCCURRENCE('Cap Screw - M8x30:4',
'Cap Screw - M8x30:4','Cap Screw - M8x30:4',#11911,#11924,
'Cap Screw - M8x30:4');
#187=NEXT_ASSEMBLY_USAGE_OCCURRENCE('Flat Washer - M8:7',
'Flat Washer - M8:7','Flat Washer - M8:7',#11911,#11939,
'Flat Washer - M8:7');
#188=NEXT_ASSEMBLY_USAGE_OCCURRENCE('Hex Nut - M8:4','Hex Nut - M8:4',
'Hex Nut - M8:4',#11911,#11940,'Hex Nut - M8:4');
#189=NEXT_ASSEMBLY_USAGE_OCCURRENCE('Flat Washer - M8:8',
'Flat Washer - M8:8','Flat Washer - M8:8',#11911,#11939,
'Flat Washer - M8:8');
#190=NEXT_ASSEMBLY_USAGE_OCCURRENCE('Cap Screw - M8x30:5',
'Cap Screw - M8x30:5','Cap Screw - M8x30:5',#11911,#11924,
'Cap Screw - M8x30:5');
#191=NEXT_ASSEMBLY_USAGE_OCCURRENCE('Flat Washer - M8:9',
'Flat Washer - M8:9','Flat Washer - M8:9',#11911,#11939,
'Flat Washer - M8:9');
#192=NEXT_ASSEMBLY_USAGE_OCCURRENCE('Hex Nut - M8:5','Hex Nut - M8:5',
'Hex Nut - M8:5',#11911,#11940,'Hex Nut - M8:5');
#193=NEXT_ASSEMBLY_USAGE_OCCURRENCE('Stepped spindle:1',
'Stepped spindle:1','Stepped spindle:1',#11925,#11926,
'Stepped spindle:1');
#194=NEXT_ASSEMBLY_USAGE_OCCURRENCE('Pulley inner spacer:1',
'Pulley inner spacer:1','Pulley inner spacer:1',#11925,#11927,
'Pulley inner spacer:1');
#195=NEXT_ASSEMBLY_USAGE_OCCURRENCE('Pulley outer spacer:1',
'Pulley outer spacer:1','Pulley outer spacer:1',#11925,#11928,
'Pulley outer spacer:1');
#196=NEXT_ASSEMBLY_USAGE_OCCURRENCE('Pulley keeper:1','Pulley keeper:1',
'Pulley keeper:1',#11925,#11929,'Pulley keeper:1');
#197=NEXT_ASSEMBLY_USAGE_OCCURRENCE('Shaft collar:1','Shaft collar:1',
'Shaft collar:1',#11925,#11930,'Shaft collar:1');
#198=NEXT_ASSEMBLY_USAGE_OCCURRENCE('Shaft collar (1):1',
'Shaft collar (1):1','Shaft collar (1):1',#11925,#11931,
'Shaft collar (1):1');
#199=NEXT_ASSEMBLY_USAGE_OCCURRENCE('Faceplate:1','Faceplate:1',
'Faceplate:1',#11925,#11932,'Faceplate:1');
#200=NEXT_ASSEMBLY_USAGE_OCCURRENCE('Drawbar keeper:1',
'Drawbar keeper:1','Drawbar keeper:1',#11925,#11933,'Drawbar keeper:1');
#201=NEXT_ASSEMBLY_USAGE_OCCURRENCE(
'Timing Pulley - 2 mm Pitch, 40 Teeth, 12 mm Bore:2',
'Timing Pulley - 2 mm Pitch, 40 Teeth, 12 mm Bore:2',
'Timing Pulley - 2 mm Pitch, 40 Teeth, 12 mm Bore:2',#11925,#11934,
'Timing Pulley - 2 mm Pitch, 40 Teeth, 12 mm Bore:2');
#202=NEXT_ASSEMBLY_USAGE_OCCURRENCE('Key 4x4x14:2','Key 4x4x14:2',
'Key 4x4x14:2',#11925,#11935,'Key 4x4x14:2');
#203=NEXT_ASSEMBLY_USAGE_OCCURRENCE('Cap Screw - M5x20:2',
'Cap Screw - M5x20:2','Cap Screw - M5x20:2',#11925,#11936,
'Cap Screw - M5x20:2');
#204=NEXT_ASSEMBLY_USAGE_OCCURRENCE('Socket Set Screw - M5x8:2',
'Socket Set Screw - M5x8:2','Socket Set Screw - M5x8:2',#11925,#11937,
'Socket Set Screw - M5x8:2');
#205=NEXT_ASSEMBLY_USAGE_OCCURRENCE('Socket Set Screw - M5x8:3',
'Socket Set Screw - M5x8:3','Socket Set Screw - M5x8:3',#11925,#11937,
'Socket Set Screw - M5x8:3');
#206=NEXT_ASSEMBLY_USAGE_OCCURRENCE('Key 6x6x20:2','Key 6x6x20:2',
'Key 6x6x20:2',#11925,#11938,'Key 6x6x20:2');
#207=NEXT_ASSEMBLY_USAGE_OCCURRENCE('Flat Washer - M8:10',
'Flat Washer - M8:10','Flat Washer - M8:10',#11925,#11939,
'Flat Washer - M8:10');
#208=NEXT_ASSEMBLY_USAGE_OCCURRENCE('Hex Nut - M8:6','Hex Nut - M8:6',
'Hex Nut - M8:6',#11925,#11940,'Hex Nut - M8:6');
#209=NEXT_ASSEMBLY_USAGE_OCCURRENCE('Flange bearing stand:1',
'Flange bearing stand:1','Flange bearing stand:1',#11910,#11911,
'Flange bearing stand:1');
#210=NEXT_ASSEMBLY_USAGE_OCCURRENCE('Stepped spindle (1):1',
'Stepped spindle (1):1','Stepped spindle (1):1',#11910,#11925,
'Stepped spindle (1):1');
#211=B_SPLINE_CURVE_WITH_KNOTS('',3,(#9556,#9557,#9558,#9559,#9560,#9561,
#9562,#9563,#9564,#9565),.UNSPECIFIED.,.F.,.F.,(4,2,2,2,4),(1.13193471301885,
1.22626174930539,1.32058878559194,1.41491753480854,1.50924628402513),
 .UNSPECIFIED.);
#212=B_SPLINE_CURVE_WITH_KNOTS('',3,(#9567,#9568,#9569,#9570,#9571,#9572,
#9573,#9574,#9575,#9576,#9577,#9578,#9579,#9580,#9581,#9582,#9583,#9584),
 .UNSPECIFIED.,.F.,.F.,(4,2,2,2,2,2,2,2,4),(0.377311571006283,0.471638607292829,
0.565965643579376,0.66029439279597,0.754623142012565,0.84895189122916,0.943280640445754,
1.0376076767323,1.13193471301885),.UNSPECIFIED.);
#213=B_SPLINE_CURVE_WITH_KNOTS('',3,(#9585,#9586,#9587,#9588,#9589,#9590,
#9591,#9592,#9593,#9594),.UNSPECIFIED.,.F.,.F.,(4,2,2,2,4),(1.50924628402513,
1.60357503324173,1.69790378245832,1.79223081874487,1.88655785503141),
 .UNSPECIFIED.);
#214=B_SPLINE_CURVE_WITH_KNOTS('',3,(#9597,#9598,#9599,#9600,#9601,#9602,
#9603,#9604,#9605,#9606,#9607,#9608,#9609,#9610,#9611,#9612,#9613,#9614,
#9615,#9616,#9617,#9618,#9619,#9620,#9621,#9622,#9623,#9624,#9625,#9626,
#9627,#9628,#9629,#9630),.UNSPECIFIED.,.T.,.F.,(4,2,2,2,2,2,2,2,2,2,2,2,
2,2,2,2,4),(0.,0.0946120580087934,0.189224116017587,0.283822945575014,0.378421775132442,
0.47302060468987,0.567619434247297,0.662231492256091,0.756843550264884,
0.851455608273677,0.94606766628247,1.0406664958399,1.13526532539733,1.22986415495475,
1.32446298451218,1.41907504252097,1.51368710052977),.UNSPECIFIED.);
#215=B_SPLINE_CURVE_WITH_KNOTS('',3,(#9633,#9634,#9635,#9636,#9637,#9638,
#9639,#9640,#9641,#9642,#9643,#9644,#9645,#9646,#9647,#9648,#9649,#9650,
#9651,#9652,#9653,#9654,#9655,#9656,#9657,#9658,#9659,#9660,#9661,#9662,
#9663,#9664,#9665,#9666),.UNSPECIFIED.,.T.,.F.,(4,2,2,2,2,2,2,2,2,2,2,2,
2,2,2,2,4),(0.,0.0946120580087934,0.189224116017587,0.283822945575014,0.378421775132442,
0.47302060468987,0.567619434247297,0.66223149225609,0.756843550264884,0.851455608273677,
0.94606766628247,1.0406664958399,1.13526532539733,1.22986415495475,1.32446298451218,
1.41907504252097,1.51368710052977),.UNSPECIFIED.);
#216=B_SPLINE_CURVE_WITH_KNOTS('',3,(#9670,#9671,#9672,#9673,#9674,#9675,
#9676,#9677,#9678,#9679),.UNSPECIFIED.,.F.,.F.,(4,2,2,2,4),(1.13193471301885,
1.22626174930539,1.32058878559194,1.41491753480854,1.50924628402513),
 .UNSPECIFIED.);
#217=B_SPLINE_CURVE_WITH_KNOTS('',3,(#9681,#9682,#9683,#9684,#9685,#9686,
#9687,#9688,#9689,#9690,#9691,#9692,#9693,#9694,#9695,#9696,#9697,#9698),
 .UNSPECIFIED.,.F.,.F.,(4,2,2,2,2,2,2,2,4),(0.377311571006283,0.47163860729283,
0.565965643579376,0.660294392795971,0.754623142012565,0.84895189122916,
0.943280640445755,1.0376076767323,1.13193471301885),.UNSPECIFIED.);
#218=B_SPLINE_CURVE_WITH_KNOTS('',3,(#9699,#9700,#9701,#9702,#9703,#9704,
#9705,#9706,#9707,#9708),.UNSPECIFIED.,.F.,.F.,(4,2,2,2,4),(1.50924628402513,
1.60357503324173,1.69790378245832,1.79223081874487,1.88655785503141),
 .UNSPECIFIED.);
#219=B_SPLINE_CURVE_WITH_KNOTS('',3,(#9717,#9718,#9719,#9720,#9721,#9722,
#9723,#9724,#9725,#9726,#9727,#9728,#9729,#9730,#9731,#9732,#9733,#9734),
 .UNSPECIFIED.,.F.,.F.,(4,2,2,2,2,2,2,2,4),(0.377311571006282,0.471638607292829,
0.565965643579376,0.660294392795971,0.754623142012565,0.84895189122916,
0.943280640445754,1.0376076767323,1.13193471301885),.UNSPECIFIED.);
#220=B_SPLINE_CURVE_WITH_KNOTS('',3,(#9736,#9737,#9738,#9739,#9740,#9741,
#9742,#9743,#9744,#9745),.UNSPECIFIED.,.F.,.F.,(4,2,2,2,4),(1.13193471301885,
1.22626174930539,1.32058878559194,1.41491753480854,1.50924628402513),
 .UNSPECIFIED.);
#221=B_SPLINE_CURVE_WITH_KNOTS('',3,(#9746,#9747,#9748,#9749,#9750,#9751,
#9752,#9753,#9754,#9755),.UNSPECIFIED.,.F.,.F.,(4,2,2,2,4),(1.50924628402513,
1.60357503324172,1.69790378245832,1.79223081874487,1.88655785503141),
 .UNSPECIFIED.);
#222=B_SPLINE_CURVE_WITH_KNOTS('',3,(#9758,#9759,#9760,#9761,#9762,#9763,
#9764,#9765,#9766,#9767,#9768,#9769,#9770,#9771,#9772,#9773,#9774,#9775),
 .UNSPECIFIED.,.F.,.F.,(4,2,2,2,2,2,2,2,4),(0.377311571006283,0.47163860729283,
0.565965643579376,0.660294392795971,0.754623142012565,0.84895189122916,
0.943280640445754,1.0376076767323,1.13193471301885),.UNSPECIFIED.);
#223=B_SPLINE_CURVE_WITH_KNOTS('',3,(#9777,#9778,#9779,#9780,#9781,#9782,
#9783,#9784,#9785,#9786),.UNSPECIFIED.,.F.,.F.,(4,2,2,2,4),(1.13193471301885,
1.22626174930539,1.32058878559194,1.41491753480854,1.50924628402513),
 .UNSPECIFIED.);
#224=B_SPLINE_CURVE_WITH_KNOTS('',3,(#9787,#9788,#9789,#9790,#9791,#9792,
#9793,#9794,#9795,#9796),.UNSPECIFIED.,.F.,.F.,(4,2,2,2,4),(1.50924628402513,
1.60357503324173,1.69790378245832,1.79223081874487,1.88655785503141),
 .UNSPECIFIED.);
#225=B_SPLINE_CURVE_WITH_KNOTS('',3,(#9799,#9800,#9801,#9802,#9803,#9804,
#9805,#9806,#9807,#9808,#9809,#9810,#9811,#9812,#9813,#9814,#9815,#9816),
 .UNSPECIFIED.,.F.,.F.,(4,2,2,2,2,2,2,2,4),(0.377311571006282,0.471638607292829,
0.565965643579376,0.66029439279597,0.754623142012565,0.84895189122916,0.943280640445754,
1.0376076767323,1.13193471301885),.UNSPECIFIED.);
#226=B_SPLINE_CURVE_WITH_KNOTS('',3,(#9818,#9819,#9820,#9821,#9822,#9823,
#9824,#9825,#9826,#9827),.UNSPECIFIED.,.F.,.F.,(4,2,2,2,4),(1.13193471301885,
1.22626174930539,1.32058878559194,1.41491753480854,1.50924628402513),
 .UNSPECIFIED.);
#227=B_SPLINE_CURVE_WITH_KNOTS('',3,(#9828,#9829,#9830,#9831,#9832,#9833,
#9834,#9835,#9836,#9837),.UNSPECIFIED.,.F.,.F.,(4,2,2,2,4),(1.50924628402513,
1.60357503324172,1.69790378245832,1.79223081874487,1.88655785503141),
 .UNSPECIFIED.);
#228=B_SPLINE_CURVE_WITH_KNOTS('',3,(#9840,#9841,#9842,#9843,#9844,#9845,
#9846,#9847,#9848,#9849,#9850,#9851,#9852,#9853,#9854,#9855,#9856,#9857),
 .UNSPECIFIED.,.F.,.F.,(4,2,2,2,2,2,2,2,4),(0.377311571006283,0.471638607292829,
0.565965643579376,0.660294392795971,0.754623142012565,0.84895189122916,
0.943280640445755,1.0376076767323,1.13193471301885),.UNSPECIFIED.);
#229=B_SPLINE_CURVE_WITH_KNOTS('',3,(#9859,#9860,#9861,#9862,#9863,#9864,
#9865,#9866,#9867,#9868),.UNSPECIFIED.,.F.,.F.,(4,2,2,2,4),(1.13193471301885,
1.22626174930539,1.32058878559194,1.41491753480854,1.50924628402513),
 .UNSPECIFIED.);
#230=B_SPLINE_CURVE_WITH_KNOTS('',3,(#9869,#9870,#9871,#9872,#9873,#9874,
#9875,#9876,#9877,#9878),.UNSPECIFIED.,.F.,.F.,(4,2,2,2,4),(1.50924628402513,
1.60357503324172,1.69790378245832,1.79223081874487,1.88655785503141),
 .UNSPECIFIED.);
#231=B_SPLINE_CURVE_WITH_KNOTS('',3,(#9882,#9883,#9884,#9885,#9886,#9887,
#9888,#9889,#9890,#9891,#9892,#9893,#9894,#9895,#9896,#9897,#9898,#9899,
#9900,#9901,#9902,#9903,#9904,#9905,#9906,#9907,#9908,#9909,#9910,#9911,
#9912,#9913,#9914,#9915),.UNSPECIFIED.,.T.,.F.,(4,2,2,2,2,2,2,2,2,2,2,2,
2,2,2,2,4),(0.,0.0946120580087934,0.189224116017587,0.283822945575014,0.378421775132442,
0.47302060468987,0.567619434247297,0.66223149225609,0.756843550264884,0.851455608273677,
0.94606766628247,1.0406664958399,1.13526532539733,1.22986415495475,1.32446298451218,
1.41907504252097,1.51368710052977),.UNSPECIFIED.);
#232=B_SPLINE_CURVE_WITH_KNOTS('',3,(#9918,#9919,#9920,#9921,#9922,#9923,
#9924,#9925,#9926,#9927,#9928,#9929,#9930,#9931,#9932,#9933,#9934,#9935,
#9936,#9937,#9938,#9939,#9940,#9941,#9942,#9943,#9944,#9945,#9946,#9947,
#9948,#9949,#9950,#9951),.UNSPECIFIED.,.T.,.F.,(4,2,2,2,2,2,2,2,2,2,2,2,
2,2,2,2,4),(0.,0.0946120580087934,0.189224116017587,0.283822945575014,0.378421775132442,
0.47302060468987,0.567619434247297,0.66223149225609,0.756843550264884,0.851455608273677,
0.94606766628247,1.0406664958399,1.13526532539733,1.22986415495475,1.32446298451218,
1.41907504252097,1.51368710052977),.UNSPECIFIED.);
#233=B_SPLINE_CURVE_WITH_KNOTS('',3,(#9956,#9957,#9958,#9959,#9960,#9961,
#9962,#9963,#9964,#9965,#9966,#9967,#9968,#9969,#9970,#9971,#9972,#9973,
#9974,#9975,#9976,#9977,#9978,#9979,#9980,#9981,#9982,#9983,#9984,#9985,
#9986,#9987,#9988,#9989),.UNSPECIFIED.,.T.,.F.,(4,2,2,2,2,2,2,2,2,2,2,2,
2,2,2,2,4),(0.,0.0946120580087934,0.189224116017587,0.283822945575014,0.378421775132442,
0.47302060468987,0.567619434247297,0.66223149225609,0.756843550264884,0.851455608273677,
0.94606766628247,1.0406664958399,1.13526532539733,1.22986415495475,1.32446298451218,
1.41907504252097,1.51368710052977),.UNSPECIFIED.);
#234=B_SPLINE_CURVE_WITH_KNOTS('',3,(#9992,#9993,#9994,#9995,#9996,#9997,
#9998,#9999,#10000,#10001,#10002,#10003,#10004,#10005,#10006,#10007,#10008,
#10009,#10010,#10011,#10012,#10013,#10014,#10015,#10016,#10017,#10018,#10019,
#10020,#10021,#10022,#10023,#10024,#10025),.UNSPECIFIED.,.T.,.F.,(4,2,2,
2,2,2,2,2,2,2,2,2,2,2,2,2,4),(0.,0.0946120580087934,0.189224116017587,0.283822945575014,
0.378421775132442,0.47302060468987,0.567619434247297,0.66223149225609,0.756843550264884,
0.851455608273677,0.94606766628247,1.0406664958399,1.13526532539733,1.22986415495475,
1.32446298451218,1.41907504252097,1.51368710052977),.UNSPECIFIED.);
#235=B_SPLINE_CURVE_WITH_KNOTS('',3,(#10248,#10249,#10250,#10251,#10252,
#10253,#10254,#10255,#10256,#10257,#10258,#10259,#10260,#10261),
 .UNSPECIFIED.,.F.,.F.,(4,2,2,2,2,2,4),(0.75600573798701,0.793568827564647,
0.872922520054201,0.952276212543756,1.03162990503331,1.11098359752287,1.1485466871005),
 .UNSPECIFIED.);
#236=B_SPLINE_CURVE_WITH_KNOTS('',3,(#10267,#10268,#10269,#10270,#10271,
#10272,#10273,#10274,#10275,#10276,#10277,#10278,#10279,#10280,#10281,#10282,
#10283,#10284),.UNSPECIFIED.,.F.,.F.,(4,2,2,2,2,2,2,2,4),(0.,0.079216580773363,
0.158433161546726,0.23764869707457,0.316864232602414,0.396079768130259,
0.475295303658103,0.554511884431466,0.633728465204829),.UNSPECIFIED.);
#237=B_SPLINE_CURVE_WITH_KNOTS('',3,(#10285,#10286,#10287,#10288,#10289,
#10290,#10291,#10292,#10293,#10294,#10295,#10296,#10297,#10298,#10299,#10300,
#10301,#10302),.UNSPECIFIED.,.F.,.F.,(4,2,2,2,2,2,2,2,4),(0.633728465204829,
0.712945045978192,0.792161626751555,0.871377162279399,0.950592697807243,
1.02980823333509,1.10902376886293,1.18824034963629,1.26745693040966),
 .UNSPECIFIED.);
#238=B_SPLINE_CURVE_WITH_KNOTS('',3,(#10305,#10306,#10307,#10308,#10309,
#10310,#10311,#10312,#10313,#10314,#10315,#10316,#10317,#10318),
 .UNSPECIFIED.,.F.,.F.,(4,2,2,2,2,2,4),(0.121154929624507,0.158718019202143,
0.238071711691697,0.317425404181252,0.396779096670807,0.476132789160362,
0.513695878737997),.UNSPECIFIED.);
#239=B_SPLINE_CURVE_WITH_KNOTS('',3,(#10343,#10344,#10345,#10346,#10347,
#10348,#10349,#10350,#10351,#10352,#10353,#10354,#10355,#10356),
 .UNSPECIFIED.,.F.,.F.,(4,2,2,2,2,2,4),(0.756005737987011,0.793568827564647,
0.872922520054201,0.952276212543756,1.03162990503331,1.11098359752287,1.1485466871005),
 .UNSPECIFIED.);
#240=B_SPLINE_CURVE_WITH_KNOTS('',3,(#10362,#10363,#10364,#10365,#10366,
#10367,#10368,#10369,#10370,#10371,#10372,#10373,#10374,#10375,#10376,#10377,
#10378,#10379),.UNSPECIFIED.,.F.,.F.,(4,2,2,2,2,2,2,2,4),(0.,0.079216580773363,
0.158433161546726,0.23764869707457,0.316864232602414,0.396079768130259,
0.475295303658103,0.554511884431466,0.633728465204829),.UNSPECIFIED.);
#241=B_SPLINE_CURVE_WITH_KNOTS('',3,(#10380,#10381,#10382,#10383,#10384,
#10385,#10386,#10387,#10388,#10389,#10390,#10391,#10392,#10393,#10394,#10395,
#10396,#10397),.UNSPECIFIED.,.F.,.F.,(4,2,2,2,2,2,2,2,4),(0.633728465204829,
0.712945045978192,0.792161626751555,0.871377162279399,0.950592697807243,
1.02980823333509,1.10902376886293,1.18824034963629,1.26745693040966),
 .UNSPECIFIED.);
#242=B_SPLINE_CURVE_WITH_KNOTS('',3,(#10400,#10401,#10402,#10403,#10404,
#10405,#10406,#10407,#10408,#10409,#10410,#10411,#10412,#10413),
 .UNSPECIFIED.,.F.,.F.,(4,2,2,2,2,2,4),(0.121154929624506,0.158718019202143,
0.238071711691697,0.317425404181252,0.396779096670807,0.476132789160362,
0.513695878737998),.UNSPECIFIED.);
#243=B_SPLINE_CURVE_WITH_KNOTS('',3,(#10553,#10554,#10555,#10556,#10557,
#10558,#10559,#10560,#10561,#10562,#10563,#10564,#10565,#10566,#10567,#10568,
#10569,#10570),.UNSPECIFIED.,.F.,.F.,(4,2,2,2,2,2,2,2,4),(0.,0.0472365751919841,
0.0944731503839683,0.14170659898184,0.188940047579712,0.236173496177583,
0.283406944775455,0.330643519967439,0.377880095159423),.UNSPECIFIED.);
#244=B_SPLINE_CURVE_WITH_KNOTS('',3,(#10571,#10572,#10573,#10574,#10575,
#10576,#10577,#10578,#10579,#10580,#10581,#10582,#10583,#10584,#10585,#10586,
#10587,#10588),.UNSPECIFIED.,.F.,.F.,(4,2,2,2,2,2,2,2,4),(0.377880095159423,
0.425116670351408,0.472353245543392,0.519586694141263,0.566820142739135,
0.614053591337007,0.661287039934879,0.708523615126863,0.755760190318847),
 .UNSPECIFIED.);
#245=B_SPLINE_CURVE_WITH_KNOTS('',3,(#10591,#10592,#10593,#10594,#10595,
#10596,#10597,#10598,#10599,#10600,#10601,#10602,#10603,#10604,#10605,#10606,
#10607,#10608),.UNSPECIFIED.,.F.,.F.,(4,2,2,2,2,2,2,2,4),(0.,0.0472365751919841,
0.0944731503839682,0.14170659898184,0.188940047579712,0.236173496177583,
0.283406944775455,0.330643519967439,0.377880095159423),.UNSPECIFIED.);
#246=B_SPLINE_CURVE_WITH_KNOTS('',3,(#10609,#10610,#10611,#10612,#10613,
#10614,#10615,#10616,#10617,#10618,#10619,#10620,#10621,#10622,#10623,#10624,
#10625,#10626),.UNSPECIFIED.,.F.,.F.,(4,2,2,2,2,2,2,2,4),(0.377880095159423,
0.425116670351408,0.472353245543392,0.519586694141263,0.566820142739135,
0.614053591337007,0.661287039934879,0.708523615126863,0.755760190318847),
 .UNSPECIFIED.);
#247=B_SPLINE_CURVE_WITH_KNOTS('',3,(#10629,#10630,#10631,#10632,#10633,
#10634,#10635,#10636,#10637,#10638,#10639,#10640,#10641,#10642,#10643,#10644,
#10645,#10646),.UNSPECIFIED.,.F.,.F.,(4,2,2,2,2,2,2,2,4),(0.,0.0472365751919841,
0.0944731503839683,0.14170659898184,0.188940047579712,0.236173496177583,
0.283406944775455,0.330643519967439,0.377880095159423),.UNSPECIFIED.);
#248=B_SPLINE_CURVE_WITH_KNOTS('',3,(#10647,#10648,#10649,#10650,#10651,
#10652,#10653,#10654,#10655,#10656,#10657,#10658,#10659,#10660,#10661,#10662,
#10663,#10664),.UNSPECIFIED.,.F.,.F.,(4,2,2,2,2,2,2,2,4),(0.377880095159423,
0.425116670351408,0.472353245543392,0.519586694141263,0.566820142739135,
0.614053591337007,0.661287039934879,0.708523615126863,0.755760190318847),
 .UNSPECIFIED.);
#249=B_SPLINE_CURVE_WITH_KNOTS('',3,(#10668,#10669,#10670,#10671,#10672,
#10673,#10674,#10675,#10676,#10677),.UNSPECIFIED.,.F.,.F.,(4,2,2,2,4),(0.565665723963061,
0.61280433739166,0.659942950820258,0.70708195805217,0.754220965284082),
 .UNSPECIFIED.);
#250=B_SPLINE_CURVE_WITH_KNOTS('',3,(#10679,#10680,#10681,#10682,#10683,
#10684,#10685,#10686,#10687,#10688,#10689,#10690,#10691,#10692,#10693,#10694,
#10695,#10696),.UNSPECIFIED.,.F.,.F.,(4,2,2,2,2,2,2,2,4),(0.18855524132102,
0.235693854749619,0.282832468178217,0.329971475410129,0.377110482642041,
0.424249489873953,0.471388497105864,0.518527110534463,0.565665723963061),
 .UNSPECIFIED.);
#251=B_SPLINE_CURVE_WITH_KNOTS('',3,(#10697,#10698,#10699,#10700,#10701,
#10702,#10703,#10704,#10705,#10706),.UNSPECIFIED.,.F.,.F.,(4,2,2,2,4),(0.754220965284082,
0.801359972515993,0.848498979747905,0.895637593176504,0.942776206605102),
 .UNSPECIFIED.);
#252=B_SPLINE_CURVE_WITH_KNOTS('',3,(#10712,#10713,#10714,#10715,#10716,
#10717,#10718,#10719,#10720,#10721),.UNSPECIFIED.,.F.,.F.,(4,2,2,2,4),(0.565665723963061,
0.61280433739166,0.659942950820258,0.70708195805217,0.754220965284082),
 .UNSPECIFIED.);
#253=B_SPLINE_CURVE_WITH_KNOTS('',3,(#10723,#10724,#10725,#10726,#10727,
#10728,#10729,#10730,#10731,#10732,#10733,#10734,#10735,#10736,#10737,#10738,
#10739,#10740),.UNSPECIFIED.,.F.,.F.,(4,2,2,2,2,2,2,2,4),(0.18855524132102,
0.235693854749619,0.282832468178217,0.329971475410129,0.377110482642041,
0.424249489873953,0.471388497105864,0.518527110534463,0.565665723963061),
 .UNSPECIFIED.);
#254=B_SPLINE_CURVE_WITH_KNOTS('',3,(#10741,#10742,#10743,#10744,#10745,
#10746,#10747,#10748,#10749,#10750),.UNSPECIFIED.,.F.,.F.,(4,2,2,2,4),(0.754220965284082,
0.801359972515993,0.848498979747905,0.895637593176504,0.942776206605102),
 .UNSPECIFIED.);
#255=B_SPLINE_CURVE_WITH_KNOTS('',3,(#10760,#10761,#10762,#10763,#10764,
#10765,#10766,#10767,#10768,#10769,#10770,#10771,#10772,#10773,#10774,#10775,
#10776,#10777),.UNSPECIFIED.,.F.,.F.,(4,2,2,2,2,2,2,2,4),(0.18855524132102,
0.235693854749619,0.282832468178217,0.329971475410129,0.377110482642041,
0.424249489873953,0.471388497105864,0.518527110534463,0.565665723963061),
 .UNSPECIFIED.);
#256=B_SPLINE_CURVE_WITH_KNOTS('',3,(#10779,#10780,#10781,#10782,#10783,
#10784,#10785,#10786,#10787,#10788),.UNSPECIFIED.,.F.,.F.,(4,2,2,2,4),(0.565665723963061,
0.61280433739166,0.659942950820258,0.70708195805217,0.754220965284082),
 .UNSPECIFIED.);
#257=B_SPLINE_CURVE_WITH_KNOTS('',3,(#10789,#10790,#10791,#10792,#10793,
#10794,#10795,#10796,#10797,#10798),.UNSPECIFIED.,.F.,.F.,(4,2,2,2,4),(0.754220965284082,
0.801359972515993,0.848498979747905,0.895637593176504,0.942776206605102),
 .UNSPECIFIED.);
#258=B_SPLINE_CURVE_WITH_KNOTS('',3,(#10801,#10802,#10803,#10804,#10805,
#10806,#10807,#10808,#10809,#10810,#10811,#10812,#10813,#10814,#10815,#10816,
#10817,#10818),.UNSPECIFIED.,.F.,.F.,(4,2,2,2,2,2,2,2,4),(0.18855524132102,
0.235693854749619,0.282832468178217,0.329971475410129,0.377110482642041,
0.424249489873953,0.471388497105864,0.518527110534463,0.565665723963061),
 .UNSPECIFIED.);
#259=B_SPLINE_CURVE_WITH_KNOTS('',3,(#10820,#10821,#10822,#10823,#10824,
#10825,#10826,#10827,#10828,#10829),.UNSPECIFIED.,.F.,.F.,(4,2,2,2,4),(0.565665723963061,
0.61280433739166,0.659942950820258,0.70708195805217,0.754220965284082),
 .UNSPECIFIED.);
#260=B_SPLINE_CURVE_WITH_KNOTS('',3,(#10830,#10831,#10832,#10833,#10834,
#10835,#10836,#10837,#10838,#10839),.UNSPECIFIED.,.F.,.F.,(4,2,2,2,4),(0.754220965284082,
0.801359972515993,0.848498979747905,0.895637593176504,0.942776206605102),
 .UNSPECIFIED.);
#261=SPHERICAL_SURFACE('',#6586,2.35);
#262=SPHERICAL_SURFACE('',#6624,2.35);
#263=CONICAL_SURFACE('',#6567,0.475,0.785398163397449);
#264=CONICAL_SURFACE('',#6571,0.485,0.785398163397448);
#265=CONICAL_SURFACE('',#6575,0.31,0.463647609000806);
#266=CONICAL_SURFACE('',#6651,0.625,0.785398163397448);
#267=CONICAL_SURFACE('',#6655,0.635,0.785398163397449);
#268=CONICAL_SURFACE('',#6659,0.41,0.463647609000806);
#269=CONICAL_SURFACE('',#6663,0.36,0.785398163397448);
#270=CONICAL_SURFACE('',#7087,0.4,0.785398163397448);
#271=CONICAL_SURFACE('',#7091,0.41,0.785398163397448);
#272=CONICAL_SURFACE('',#7095,0.26,0.463647609000806);
#273=CONICAL_SURFACE('',#7099,0.225,0.785398163397448);
#274=CONICAL_SURFACE('',#7120,0.235,0.785398163397448);
#275=CONICAL_SURFACE('',#7124,0.2125,0.785398163397448);
#276=CONICAL_SURFACE('',#7148,0.734027674973257,1.0471975511966);
#277=CONICAL_SURFACE('',#7150,0.734027674973257,1.0471975511966);
#278=ORIENTED_CLOSED_SHELL('',*,#6138,.F.);
#279=ORIENTED_CLOSED_SHELL('',*,#6144,.F.);
#280=ORIENTED_CLOSED_SHELL('',*,#6156,.F.);
#281=BREP_WITH_VOIDS('Body1',#6139,(#278));
#282=BREP_WITH_VOIDS('Body1',#6143,(#279));
#283=BREP_WITH_VOIDS('Body1',#6155,(#280));
#284=SHAPE_REPRESENTATION_RELATIONSHIP('SRR','None',#11880,#311);
#285=SHAPE_REPRESENTATION_RELATIONSHIP('SRR','None',#11881,#312);
#286=SHAPE_REPRESENTATION_RELATIONSHIP('SRR','None',#11882,#313);
#287=SHAPE_REPRESENTATION_RELATIONSHIP('SRR','None',#11883,#314);
#288=SHAPE_REPRESENTATION_RELATIONSHIP('SRR','None',#11884,#315);
#289=SHAPE_REPRESENTATION_RELATIONSHIP('SRR','None',#11885,#316);
#290=SHAPE_REPRESENTATION_RELATIONSHIP('SRR','None',#11886,#317);
#291=SHAPE_REPRESENTATION_RELATIONSHIP('SRR','None',#11887,#318);
#292=SHAPE_REPRESENTATION_RELATIONSHIP('SRR','None',#11888,#319);
#293=SHAPE_REPRESENTATION_RELATIONSHIP('SRR','None',#11890,#320);
#294=SHAPE_REPRESENTATION_RELATIONSHIP('SRR','None',#11891,#321);
#295=SHAPE_REPRESENTATION_RELATIONSHIP('SRR','None',#11892,#322);
#296=SHAPE_REPRESENTATION_RELATIONSHIP('SRR','None',#11894,#323);
#297=SHAPE_REPRESENTATION_RELATIONSHIP('SRR','None',#11895,#324);
#298=SHAPE_REPRESENTATION_RELATIONSHIP('SRR','None',#11896,#325);
#299=SHAPE_REPRESENTATION_RELATIONSHIP('SRR','None',#11897,#326);
#300=SHAPE_REPRESENTATION_RELATIONSHIP('SRR','None',#11898,#327);
#301=SHAPE_REPRESENTATION_RELATIONSHIP('SRR','None',#11899,#328);
#302=SHAPE_REPRESENTATION_RELATIONSHIP('SRR','None',#11900,#329);
#303=SHAPE_REPRESENTATION_RELATIONSHIP('SRR','None',#11901,#330);
#304=SHAPE_REPRESENTATION_RELATIONSHIP('SRR','None',#11902,#331);
#305=SHAPE_REPRESENTATION_RELATIONSHIP('SRR','None',#11903,#332);
#306=SHAPE_REPRESENTATION_RELATIONSHIP('SRR','None',#11904,#333);
#307=SHAPE_REPRESENTATION_RELATIONSHIP('SRR','None',#11905,#334);
#308=SHAPE_REPRESENTATION_RELATIONSHIP('SRR','None',#11906,#335);
#309=SHAPE_REPRESENTATION_RELATIONSHIP('SRR','None',#11907,#336);
#310=SHAPE_REPRESENTATION_RELATIONSHIP('SRR','None',#11908,#337);
#311=ADVANCED_BREP_SHAPE_REPRESENTATION('',(#366),#11735);
#312=ADVANCED_BREP_SHAPE_REPRESENTATION('',(#367),#11736);
#313=ADVANCED_BREP_SHAPE_REPRESENTATION('',(#368),#11737);
#314=ADVANCED_BREP_SHAPE_REPRESENTATION('',(#369),#11738);
#315=ADVANCED_BREP_SHAPE_REPRESENTATION('',(#370),#11739);
#316=ADVANCED_BREP_SHAPE_REPRESENTATION('',(#371),#11740);
#317=ADVANCED_BREP_SHAPE_REPRESENTATION('',(#372),#11741);
#318=ADVANCED_BREP_SHAPE_REPRESENTATION('',(#373),#11742);
#319=ADVANCED_BREP_SHAPE_REPRESENTATION('',(#281),#11743);
#320=ADVANCED_BREP_SHAPE_REPRESENTATION('',(#374),#11745);
#321=ADVANCED_BREP_SHAPE_REPRESENTATION('',(#375,#376),#11746);
#322=ADVANCED_BREP_SHAPE_REPRESENTATION('',(#282),#11747);
#323=ADVANCED_BREP_SHAPE_REPRESENTATION('',(#377),#11749);
#324=ADVANCED_BREP_SHAPE_REPRESENTATION('',(#378),#11750);
#325=ADVANCED_BREP_SHAPE_REPRESENTATION('',(#379),#11751);
#326=ADVANCED_BREP_SHAPE_REPRESENTATION('',(#380),#11752);
#327=ADVANCED_BREP_SHAPE_REPRESENTATION('',(#381),#11753);
#328=ADVANCED_BREP_SHAPE_REPRESENTATION('',(#382),#11754);
#329=ADVANCED_BREP_SHAPE_REPRESENTATION('',(#383),#11755);
#330=ADVANCED_BREP_SHAPE_REPRESENTATION('',(#384),#11756);
#331=ADVANCED_BREP_SHAPE_REPRESENTATION('',(#385),#11757);
#332=ADVANCED_BREP_SHAPE_REPRESENTATION('',(#386),#11758);
#333=ADVANCED_BREP_SHAPE_REPRESENTATION('',(#283),#11759);
#334=ADVANCED_BREP_SHAPE_REPRESENTATION('',(#387),#11760);
#335=ADVANCED_BREP_SHAPE_REPRESENTATION('',(#388),#11761);
#336=ADVANCED_BREP_SHAPE_REPRESENTATION('',(#389),#11762);
#337=ADVANCED_BREP_SHAPE_REPRESENTATION('',(#390),#11763);
#338=STYLED_ITEM('',(#12078),#366);
#339=STYLED_ITEM('',(#12099),#367);
#340=STYLED_ITEM('',(#12113),#368);
#341=STYLED_ITEM('',(#12113),#369);
#342=STYLED_ITEM('',(#12113),#370);
#343=STYLED_ITEM('',(#12113),#371);
#344=STYLED_ITEM('',(#12092),#372);
#345=STYLED_ITEM('',(#12092),#373);
#346=STYLED_ITEM('',(#12106),#281);
#347=STYLED_ITEM('',(#12078),#374);
#348=STYLED_ITEM('',(#12099),#375);
#349=STYLED_ITEM('',(#12099),#376);
#350=STYLED_ITEM('',(#12106),#282);
#351=STYLED_ITEM('',(#12085),#377);
#352=STYLED_ITEM('',(#12113),#378);
#353=STYLED_ITEM('',(#12085),#379);
#354=STYLED_ITEM('',(#12113),#380);
#355=STYLED_ITEM('',(#12099),#381);
#356=STYLED_ITEM('',(#12099),#382);
#357=STYLED_ITEM('',(#12085),#383);
#358=STYLED_ITEM('',(#12092),#384);
#359=STYLED_ITEM('',(#12092),#385);
#360=STYLED_ITEM('',(#12099),#386);
#361=STYLED_ITEM('',(#12106),#283);
#362=STYLED_ITEM('',(#12106),#387);
#363=STYLED_ITEM('',(#12099),#388);
#364=STYLED_ITEM('',(#12106),#389);
#365=STYLED_ITEM('',(#12106),#390);
#366=MANIFOLD_SOLID_BREP('Body1',#6130);
#367=MANIFOLD_SOLID_BREP('Body1',#6131);
#368=MANIFOLD_SOLID_BREP('Body1',#6132);
#369=MANIFOLD_SOLID_BREP('Body1',#6133);
#370=MANIFOLD_SOLID_BREP('Body1',#6134);
#371=MANIFOLD_SOLID_BREP('Body1',#6135);
#372=MANIFOLD_SOLID_BREP('Body1',#6136);
#373=MANIFOLD_SOLID_BREP('Body1',#6137);
#374=MANIFOLD_SOLID_BREP('Body1',#6140);
#375=MANIFOLD_SOLID_BREP('Body1',#6141);
#376=MANIFOLD_SOLID_BREP('Body2',#6142);
#377=MANIFOLD_SOLID_BREP('Body1',#6145);
#378=MANIFOLD_SOLID_BREP('Body1',#6146);
#379=MANIFOLD_SOLID_BREP('Body1',#6147);
#380=MANIFOLD_SOLID_BREP('Body1',#6148);
#381=MANIFOLD_SOLID_BREP('Body1',#6149);
#382=MANIFOLD_SOLID_BREP('Body1',#6150);
#383=MANIFOLD_SOLID_BREP('Body1',#6151);
#384=MANIFOLD_SOLID_BREP('Body1',#6152);
#385=MANIFOLD_SOLID_BREP('Body1',#6153);
#386=MANIFOLD_SOLID_BREP('Body1',#6154);
#387=MANIFOLD_SOLID_BREP('Body1',#6157);
#388=MANIFOLD_SOLID_BREP('Body1',#6158);
#389=MANIFOLD_SOLID_BREP('Body1',#6159);
#390=MANIFOLD_SOLID_BREP('Body1',#6160);
#391=FACE_BOUND('',#1026,.T.);
#392=FACE_BOUND('',#1027,.T.);
#393=FACE_BOUND('',#1029,.T.);
#394=FACE_BOUND('',#1030,.T.);
#395=FACE_BOUND('',#1039,.T.);
#396=FACE_BOUND('',#1040,.T.);
#397=FACE_BOUND('',#1043,.T.);
#398=FACE_BOUND('',#1044,.T.);
#399=FACE_BOUND('',#1045,.T.);
#400=FACE_BOUND('',#1046,.T.);
#401=FACE_BOUND('',#1047,.T.);
#402=FACE_BOUND('',#1051,.T.);
#403=FACE_BOUND('',#1052,.T.);
#404=FACE_BOUND('',#1053,.T.);
#405=FACE_BOUND('',#1054,.T.);
#406=FACE_BOUND('',#1055,.T.);
#407=FACE_BOUND('',#1058,.T.);
#408=FACE_BOUND('',#1059,.T.);
#409=FACE_BOUND('',#1063,.T.);
#410=FACE_BOUND('',#1065,.T.);
#411=FACE_BOUND('',#1069,.T.);
#412=FACE_BOUND('',#1071,.T.);
#413=FACE_BOUND('',#1075,.T.);
#414=FACE_BOUND('',#1077,.T.);
#415=FACE_BOUND('',#1081,.T.);
#416=FACE_BOUND('',#1083,.T.);
#417=FACE_BOUND('',#1110,.T.);
#418=FACE_BOUND('',#1116,.T.);
#419=FACE_BOUND('',#1117,.T.);
#420=FACE_BOUND('',#1121,.T.);
#421=FACE_BOUND('',#1123,.T.);
#422=FACE_BOUND('',#1137,.T.);
#423=FACE_BOUND('',#1138,.T.);
#424=FACE_BOUND('',#1139,.T.);
#425=FACE_BOUND('',#1140,.T.);
#426=FACE_BOUND('',#1141,.T.);
#427=FACE_BOUND('',#1143,.T.);
#428=FACE_BOUND('',#1144,.T.);
#429=FACE_BOUND('',#1145,.T.);
#430=FACE_BOUND('',#1146,.T.);
#431=FACE_BOUND('',#1147,.T.);
#432=FACE_BOUND('',#1150,.T.);
#433=FACE_BOUND('',#1152,.T.);
#434=FACE_BOUND('',#1153,.T.);
#435=FACE_BOUND('',#1155,.T.);
#436=FACE_BOUND('',#1159,.T.);
#437=FACE_BOUND('',#1160,.T.);
#438=FACE_BOUND('',#1161,.T.);
#439=FACE_BOUND('',#1162,.T.);
#440=FACE_BOUND('',#1163,.T.);
#441=FACE_BOUND('',#1164,.T.);
#442=FACE_BOUND('',#1170,.T.);
#443=FACE_BOUND('',#1172,.T.);
#444=FACE_BOUND('',#1175,.T.);
#445=FACE_BOUND('',#1177,.T.);
#446=FACE_BOUND('',#1178,.T.);
#447=FACE_BOUND('',#1179,.T.);
#448=FACE_BOUND('',#1180,.T.);
#449=FACE_BOUND('',#1181,.T.);
#450=FACE_BOUND('',#1182,.T.);
#451=FACE_BOUND('',#1188,.T.);
#452=FACE_BOUND('',#1216,.T.);
#453=FACE_BOUND('',#1218,.T.);
#454=FACE_BOUND('',#1220,.T.);
#455=FACE_BOUND('',#1222,.T.);
#456=FACE_BOUND('',#1224,.T.);
#457=FACE_BOUND('',#1228,.T.);
#458=FACE_BOUND('',#1230,.T.);
#459=FACE_BOUND('',#1234,.T.);
#460=FACE_BOUND('',#1236,.T.);
#461=FACE_BOUND('',#1240,.T.);
#462=FACE_BOUND('',#1242,.T.);
#463=FACE_BOUND('',#1247,.T.);
#464=FACE_BOUND('',#1249,.T.);
#465=FACE_BOUND('',#1251,.T.);
#466=FACE_BOUND('',#1253,.T.);
#467=FACE_BOUND('',#1258,.T.);
#468=FACE_BOUND('',#1260,.T.);
#469=FACE_BOUND('',#1262,.T.);
#470=FACE_BOUND('',#1264,.T.);
#471=FACE_BOUND('',#1269,.T.);
#472=FACE_BOUND('',#1270,.T.);
#473=FACE_BOUND('',#1271,.T.);
#474=FACE_BOUND('',#1272,.T.);
#475=FACE_BOUND('',#1273,.T.);
#476=FACE_BOUND('',#1274,.T.);
#477=FACE_BOUND('',#1275,.T.);
#478=FACE_BOUND('',#1284,.T.);
#479=FACE_BOUND('',#1285,.T.);
#480=FACE_BOUND('',#1286,.T.);
#481=FACE_BOUND('',#1287,.T.);
#482=FACE_BOUND('',#1288,.T.);
#483=FACE_BOUND('',#1289,.T.);
#484=FACE_BOUND('',#1290,.T.);
#485=FACE_BOUND('',#1294,.T.);
#486=FACE_BOUND('',#1298,.T.);
#487=FACE_BOUND('',#1300,.T.);
#488=FACE_BOUND('',#1303,.T.);
#489=FACE_BOUND('',#1306,.T.);
#490=FACE_BOUND('',#1308,.T.);
#491=FACE_BOUND('',#1309,.T.);
#492=FACE_BOUND('',#1310,.T.);
#493=FACE_BOUND('',#1314,.T.);
#494=FACE_BOUND('',#1315,.T.);
#495=FACE_BOUND('',#1316,.T.);
#496=FACE_BOUND('',#1320,.T.);
#497=FACE_BOUND('',#1322,.T.);
#498=FACE_BOUND('',#1325,.T.);
#499=FACE_BOUND('',#1327,.T.);
#500=FACE_BOUND('',#1424,.T.);
#501=FACE_BOUND('',#1445,.T.);
#502=FACE_BOUND('',#1463,.T.);
#503=FACE_BOUND('',#1465,.T.);
#504=FACE_BOUND('',#1476,.T.);
#505=FACE_BOUND('',#1478,.T.);
#506=PLANE('',#6468);
#507=PLANE('',#6469);
#508=PLANE('',#6470);
#509=PLANE('',#6471);
#510=PLANE('',#6472);
#511=PLANE('',#6473);
#512=PLANE('',#6496);
#513=PLANE('',#6497);
#514=PLANE('',#6498);
#515=PLANE('',#6499);
#516=PLANE('',#6500);
#517=PLANE('',#6501);
#518=PLANE('',#6502);
#519=PLANE('',#6503);
#520=PLANE('',#6511);
#521=PLANE('',#6512);
#522=PLANE('',#6520);
#523=PLANE('',#6521);
#524=PLANE('',#6529);
#525=PLANE('',#6530);
#526=PLANE('',#6538);
#527=PLANE('',#6539);
#528=PLANE('',#6541);
#529=PLANE('',#6542);
#530=PLANE('',#6543);
#531=PLANE('',#6544);
#532=PLANE('',#6545);
#533=PLANE('',#6546);
#534=PLANE('',#6548);
#535=PLANE('',#6549);
#536=PLANE('',#6550);
#537=PLANE('',#6551);
#538=PLANE('',#6552);
#539=PLANE('',#6553);
#540=PLANE('',#6555);
#541=PLANE('',#6556);
#542=PLANE('',#6557);
#543=PLANE('',#6558);
#544=PLANE('',#6559);
#545=PLANE('',#6560);
#546=PLANE('',#6561);
#547=PLANE('',#6562);
#548=PLANE('',#6563);
#549=PLANE('',#6565);
#550=PLANE('',#6573);
#551=PLANE('',#6594);
#552=PLANE('',#6595);
#553=PLANE('',#6608);
#554=PLANE('',#6609);
#555=PLANE('',#6610);
#556=PLANE('',#6611);
#557=PLANE('',#6612);
#558=PLANE('',#6613);
#559=PLANE('',#6614);
#560=PLANE('',#6615);
#561=PLANE('',#6616);
#562=PLANE('',#6617);
#563=PLANE('',#6622);
#564=PLANE('',#6627);
#565=PLANE('',#6637);
#566=PLANE('',#6639);
#567=PLANE('',#6643);
#568=PLANE('',#6649);
#569=PLANE('',#6657);
#570=PLANE('',#6665);
#571=PLANE('',#6666);
#572=PLANE('',#6667);
#573=PLANE('',#6668);
#574=PLANE('',#6669);
#575=PLANE('',#6670);
#576=PLANE('',#6671);
#577=PLANE('',#6672);
#578=PLANE('',#6673);
#579=PLANE('',#6676);
#580=PLANE('',#6677);
#581=PLANE('',#6679);
#582=PLANE('',#6680);
#583=PLANE('',#6681);
#584=PLANE('',#6686);
#585=PLANE('',#6687);
#586=PLANE('',#6688);
#587=PLANE('',#6690);
#588=PLANE('',#6691);
#589=PLANE('',#6692);
#590=PLANE('',#6697);
#591=PLANE('',#6701);
#592=PLANE('',#6705);
#593=PLANE('',#6706);
#594=PLANE('',#6714);
#595=PLANE('',#6715);
#596=PLANE('',#6723);
#597=PLANE('',#6724);
#598=PLANE('',#6732);
#599=PLANE('',#6733);
#600=PLANE('',#6735);
#601=PLANE('',#6740);
#602=PLANE('',#6747);
#603=PLANE('',#6748);
#604=PLANE('',#6750);
#605=PLANE('',#6755);
#606=PLANE('',#6762);
#607=PLANE('',#6763);
#608=PLANE('',#6765);
#609=PLANE('',#6766);
#610=PLANE('',#6767);
#611=PLANE('',#6768);
#612=PLANE('',#6791);
#613=PLANE('',#6797);
#614=PLANE('',#6805);
#615=PLANE('',#6806);
#616=PLANE('',#6808);
#617=PLANE('',#6809);
#618=PLANE('',#6811);
#619=PLANE('',#6812);
#620=PLANE('',#6824);
#621=PLANE('',#6825);
#622=PLANE('',#6909);
#623=PLANE('',#6910);
#624=PLANE('',#7074);
#625=PLANE('',#7075);
#626=PLANE('',#7076);
#627=PLANE('',#7077);
#628=PLANE('',#7078);
#629=PLANE('',#7079);
#630=PLANE('',#7080);
#631=PLANE('',#7081);
#632=PLANE('',#7082);
#633=PLANE('',#7083);
#634=PLANE('',#7085);
#635=PLANE('',#7093);
#636=PLANE('',#7101);
#637=PLANE('',#7102);
#638=PLANE('',#7103);
#639=PLANE('',#7104);
#640=PLANE('',#7105);
#641=PLANE('',#7106);
#642=PLANE('',#7107);
#643=PLANE('',#7108);
#644=PLANE('',#7109);
#645=PLANE('',#7111);
#646=PLANE('',#7112);
#647=PLANE('',#7113);
#648=PLANE('',#7114);
#649=PLANE('',#7115);
#650=PLANE('',#7116);
#651=PLANE('',#7117);
#652=PLANE('',#7118);
#653=PLANE('',#7126);
#654=PLANE('',#7128);
#655=PLANE('',#7129);
#656=PLANE('',#7130);
#657=PLANE('',#7131);
#658=PLANE('',#7132);
#659=PLANE('',#7133);
#660=PLANE('',#7134);
#661=PLANE('',#7135);
#662=PLANE('',#7136);
#663=PLANE('',#7137);
#664=PLANE('',#7145);
#665=PLANE('',#7146);
#666=PLANE('',#7152);
#667=PLANE('',#7153);
#668=PLANE('',#7154);
#669=PLANE('',#7158);
#670=PLANE('',#7159);
#671=PLANE('',#7160);
#672=PLANE('',#7161);
#673=PLANE('',#7162);
#674=FACE_OUTER_BOUND('',#1019,.T.);
#675=FACE_OUTER_BOUND('',#1020,.T.);
#676=FACE_OUTER_BOUND('',#1021,.T.);
#677=FACE_OUTER_BOUND('',#1022,.T.);
#678=FACE_OUTER_BOUND('',#1023,.T.);
#679=FACE_OUTER_BOUND('',#1024,.T.);
#680=FACE_OUTER_BOUND('',#1025,.T.);
#681=FACE_OUTER_BOUND('',#1028,.T.);
#682=FACE_OUTER_BOUND('',#1031,.T.);
#683=FACE_OUTER_BOUND('',#1032,.T.);
#684=FACE_OUTER_BOUND('',#1033,.T.);
#685=FACE_OUTER_BOUND('',#1034,.T.);
#686=FACE_OUTER_BOUND('',#1035,.T.);
#687=FACE_OUTER_BOUND('',#1036,.T.);
#688=FACE_OUTER_BOUND('',#1037,.T.);
#689=FACE_OUTER_BOUND('',#1038,.T.);
#690=FACE_OUTER_BOUND('',#1041,.T.);
#691=FACE_OUTER_BOUND('',#1042,.T.);
#692=FACE_OUTER_BOUND('',#1048,.T.);
#693=FACE_OUTER_BOUND('',#1049,.T.);
#694=FACE_OUTER_BOUND('',#1050,.T.);
#695=FACE_OUTER_BOUND('',#1056,.T.);
#696=FACE_OUTER_BOUND('',#1057,.T.);
#697=FACE_OUTER_BOUND('',#1060,.T.);
#698=FACE_OUTER_BOUND('',#1061,.T.);
#699=FACE_OUTER_BOUND('',#1062,.T.);
#700=FACE_OUTER_BOUND('',#1064,.T.);
#701=FACE_OUTER_BOUND('',#1066,.T.);
#702=FACE_OUTER_BOUND('',#1067,.T.);
#703=FACE_OUTER_BOUND('',#1068,.T.);
#704=FACE_OUTER_BOUND('',#1070,.T.);
#705=FACE_OUTER_BOUND('',#1072,.T.);
#706=FACE_OUTER_BOUND('',#1073,.T.);
#707=FACE_OUTER_BOUND('',#1074,.T.);
#708=FACE_OUTER_BOUND('',#1076,.T.);
#709=FACE_OUTER_BOUND('',#1078,.T.);
#710=FACE_OUTER_BOUND('',#1079,.T.);
#711=FACE_OUTER_BOUND('',#1080,.T.);
#712=FACE_OUTER_BOUND('',#1082,.T.);
#713=FACE_OUTER_BOUND('',#1084,.T.);
#714=FACE_OUTER_BOUND('',#1085,.T.);
#715=FACE_OUTER_BOUND('',#1086,.T.);
#716=FACE_OUTER_BOUND('',#1087,.T.);
#717=FACE_OUTER_BOUND('',#1088,.T.);
#718=FACE_OUTER_BOUND('',#1089,.T.);
#719=FACE_OUTER_BOUND('',#1090,.T.);
#720=FACE_OUTER_BOUND('',#1091,.T.);
#721=FACE_OUTER_BOUND('',#1092,.T.);
#722=FACE_OUTER_BOUND('',#1093,.T.);
#723=FACE_OUTER_BOUND('',#1094,.T.);
#724=FACE_OUTER_BOUND('',#1095,.T.);
#725=FACE_OUTER_BOUND('',#1096,.T.);
#726=FACE_OUTER_BOUND('',#1097,.T.);
#727=FACE_OUTER_BOUND('',#1098,.T.);
#728=FACE_OUTER_BOUND('',#1099,.T.);
#729=FACE_OUTER_BOUND('',#1100,.T.);
#730=FACE_OUTER_BOUND('',#1101,.T.);
#731=FACE_OUTER_BOUND('',#1102,.T.);
#732=FACE_OUTER_BOUND('',#1103,.T.);
#733=FACE_OUTER_BOUND('',#1104,.T.);
#734=FACE_OUTER_BOUND('',#1105,.T.);
#735=FACE_OUTER_BOUND('',#1106,.T.);
#736=FACE_OUTER_BOUND('',#1107,.T.);
#737=FACE_OUTER_BOUND('',#1108,.T.);
#738=FACE_OUTER_BOUND('',#1109,.T.);
#739=FACE_OUTER_BOUND('',#1111,.T.);
#740=FACE_OUTER_BOUND('',#1112,.T.);
#741=FACE_OUTER_BOUND('',#1113,.T.);
#742=FACE_OUTER_BOUND('',#1114,.T.);
#743=FACE_OUTER_BOUND('',#1115,.T.);
#744=FACE_OUTER_BOUND('',#1118,.T.);
#745=FACE_OUTER_BOUND('',#1119,.T.);
#746=FACE_OUTER_BOUND('',#1120,.T.);
#747=FACE_OUTER_BOUND('',#1122,.T.);
#748=FACE_OUTER_BOUND('',#1124,.T.);
#749=FACE_OUTER_BOUND('',#1125,.T.);
#750=FACE_OUTER_BOUND('',#1126,.T.);
#751=FACE_OUTER_BOUND('',#1127,.T.);
#752=FACE_OUTER_BOUND('',#1128,.T.);
#753=FACE_OUTER_BOUND('',#1129,.T.);
#754=FACE_OUTER_BOUND('',#1130,.T.);
#755=FACE_OUTER_BOUND('',#1131,.T.);
#756=FACE_OUTER_BOUND('',#1132,.T.);
#757=FACE_OUTER_BOUND('',#1133,.T.);
#758=FACE_OUTER_BOUND('',#1134,.T.);
#759=FACE_OUTER_BOUND('',#1135,.T.);
#760=FACE_OUTER_BOUND('',#1136,.T.);
#761=FACE_OUTER_BOUND('',#1142,.T.);
#762=FACE_OUTER_BOUND('',#1148,.T.);
#763=FACE_OUTER_BOUND('',#1149,.T.);
#764=FACE_OUTER_BOUND('',#1151,.T.);
#765=FACE_OUTER_BOUND('',#1154,.T.);
#766=FACE_OUTER_BOUND('',#1156,.T.);
#767=FACE_OUTER_BOUND('',#1157,.T.);
#768=FACE_OUTER_BOUND('',#1158,.T.);
#769=FACE_OUTER_BOUND('',#1165,.T.);
#770=FACE_OUTER_BOUND('',#1166,.T.);
#771=FACE_OUTER_BOUND('',#1167,.T.);
#772=FACE_OUTER_BOUND('',#1168,.T.);
#773=FACE_OUTER_BOUND('',#1169,.T.);
#774=FACE_OUTER_BOUND('',#1171,.T.);
#775=FACE_OUTER_BOUND('',#1173,.T.);
#776=FACE_OUTER_BOUND('',#1174,.T.);
#777=FACE_OUTER_BOUND('',#1176,.T.);
#778=FACE_OUTER_BOUND('',#1183,.T.);
#779=FACE_OUTER_BOUND('',#1184,.T.);
#780=FACE_OUTER_BOUND('',#1185,.T.);
#781=FACE_OUTER_BOUND('',#1186,.T.);
#782=FACE_OUTER_BOUND('',#1187,.T.);
#783=FACE_OUTER_BOUND('',#1189,.T.);
#784=FACE_OUTER_BOUND('',#1190,.T.);
#785=FACE_OUTER_BOUND('',#1191,.T.);
#786=FACE_OUTER_BOUND('',#1192,.T.);
#787=FACE_OUTER_BOUND('',#1193,.T.);
#788=FACE_OUTER_BOUND('',#1194,.T.);
#789=FACE_OUTER_BOUND('',#1195,.T.);
#790=FACE_OUTER_BOUND('',#1196,.T.);
#791=FACE_OUTER_BOUND('',#1197,.T.);
#792=FACE_OUTER_BOUND('',#1198,.T.);
#793=FACE_OUTER_BOUND('',#1199,.T.);
#794=FACE_OUTER_BOUND('',#1200,.T.);
#795=FACE_OUTER_BOUND('',#1201,.T.);
#796=FACE_OUTER_BOUND('',#1202,.T.);
#797=FACE_OUTER_BOUND('',#1203,.T.);
#798=FACE_OUTER_BOUND('',#1204,.T.);
#799=FACE_OUTER_BOUND('',#1205,.T.);
#800=FACE_OUTER_BOUND('',#1206,.T.);
#801=FACE_OUTER_BOUND('',#1207,.T.);
#802=FACE_OUTER_BOUND('',#1208,.T.);
#803=FACE_OUTER_BOUND('',#1209,.T.);
#804=FACE_OUTER_BOUND('',#1210,.T.);
#805=FACE_OUTER_BOUND('',#1211,.T.);
#806=FACE_OUTER_BOUND('',#1212,.T.);
#807=FACE_OUTER_BOUND('',#1213,.T.);
#808=FACE_OUTER_BOUND('',#1214,.T.);
#809=FACE_OUTER_BOUND('',#1215,.T.);
#810=FACE_OUTER_BOUND('',#1217,.T.);
#811=FACE_OUTER_BOUND('',#1219,.T.);
#812=FACE_OUTER_BOUND('',#1221,.T.);
#813=FACE_OUTER_BOUND('',#1223,.T.);
#814=FACE_OUTER_BOUND('',#1225,.T.);
#815=FACE_OUTER_BOUND('',#1226,.T.);
#816=FACE_OUTER_BOUND('',#1227,.T.);
#817=FACE_OUTER_BOUND('',#1229,.T.);
#818=FACE_OUTER_BOUND('',#1231,.T.);
#819=FACE_OUTER_BOUND('',#1232,.T.);
#820=FACE_OUTER_BOUND('',#1233,.T.);
#821=FACE_OUTER_BOUND('',#1235,.T.);
#822=FACE_OUTER_BOUND('',#1237,.T.);
#823=FACE_OUTER_BOUND('',#1238,.T.);
#824=FACE_OUTER_BOUND('',#1239,.T.);
#825=FACE_OUTER_BOUND('',#1241,.T.);
#826=FACE_OUTER_BOUND('',#1243,.T.);
#827=FACE_OUTER_BOUND('',#1244,.T.);
#828=FACE_OUTER_BOUND('',#1245,.T.);
#829=FACE_OUTER_BOUND('',#1246,.T.);
#830=FACE_OUTER_BOUND('',#1248,.T.);
#831=FACE_OUTER_BOUND('',#1250,.T.);
#832=FACE_OUTER_BOUND('',#1252,.T.);
#833=FACE_OUTER_BOUND('',#1254,.T.);
#834=FACE_OUTER_BOUND('',#1255,.T.);
#835=FACE_OUTER_BOUND('',#1256,.T.);
#836=FACE_OUTER_BOUND('',#1257,.T.);
#837=FACE_OUTER_BOUND('',#1259,.T.);
#838=FACE_OUTER_BOUND('',#1261,.T.);
#839=FACE_OUTER_BOUND('',#1263,.T.);
#840=FACE_OUTER_BOUND('',#1265,.T.);
#841=FACE_OUTER_BOUND('',#1266,.T.);
#842=FACE_OUTER_BOUND('',#1267,.T.);
#843=FACE_OUTER_BOUND('',#1268,.T.);
#844=FACE_OUTER_BOUND('',#1276,.T.);
#845=FACE_OUTER_BOUND('',#1277,.T.);
#846=FACE_OUTER_BOUND('',#1278,.T.);
#847=FACE_OUTER_BOUND('',#1279,.T.);
#848=FACE_OUTER_BOUND('',#1280,.T.);
#849=FACE_OUTER_BOUND('',#1281,.T.);
#850=FACE_OUTER_BOUND('',#1282,.T.);
#851=FACE_OUTER_BOUND('',#1283,.T.);
#852=FACE_OUTER_BOUND('',#1291,.T.);
#853=FACE_OUTER_BOUND('',#1292,.T.);
#854=FACE_OUTER_BOUND('',#1293,.T.);
#855=FACE_OUTER_BOUND('',#1295,.T.);
#856=FACE_OUTER_BOUND('',#1296,.T.);
#857=FACE_OUTER_BOUND('',#1297,.T.);
#858=FACE_OUTER_BOUND('',#1299,.T.);
#859=FACE_OUTER_BOUND('',#1301,.T.);
#860=FACE_OUTER_BOUND('',#1302,.T.);
#861=FACE_OUTER_BOUND('',#1304,.T.);
#862=FACE_OUTER_BOUND('',#1305,.T.);
#863=FACE_OUTER_BOUND('',#1307,.T.);
#864=FACE_OUTER_BOUND('',#1311,.T.);
#865=FACE_OUTER_BOUND('',#1312,.T.);
#866=FACE_OUTER_BOUND('',#1313,.T.);
#867=FACE_OUTER_BOUND('',#1317,.T.);
#868=FACE_OUTER_BOUND('',#1318,.T.);
#869=FACE_OUTER_BOUND('',#1319,.T.);
#870=FACE_OUTER_BOUND('',#1321,.T.);
#871=FACE_OUTER_BOUND('',#1323,.T.);
#872=FACE_OUTER_BOUND('',#1324,.T.);
#873=FACE_OUTER_BOUND('',#1326,.T.);
#874=FACE_OUTER_BOUND('',#1328,.T.);
#875=FACE_OUTER_BOUND('',#1329,.T.);
#876=FACE_OUTER_BOUND('',#1330,.T.);
#877=FACE_OUTER_BOUND('',#1331,.T.);
#878=FACE_OUTER_BOUND('',#1332,.T.);
#879=FACE_OUTER_BOUND('',#1333,.T.);
#880=FACE_OUTER_BOUND('',#1334,.T.);
#881=FACE_OUTER_BOUND('',#1335,.T.);
#882=FACE_OUTER_BOUND('',#1336,.T.);
#883=FACE_OUTER_BOUND('',#1337,.T.);
#884=FACE_OUTER_BOUND('',#1338,.T.);
#885=FACE_OUTER_BOUND('',#1339,.T.);
#886=FACE_OUTER_BOUND('',#1340,.T.);
#887=FACE_OUTER_BOUND('',#1341,.T.);
#888=FACE_OUTER_BOUND('',#1342,.T.);
#889=FACE_OUTER_BOUND('',#1343,.T.);
#890=FACE_OUTER_BOUND('',#1344,.T.);
#891=FACE_OUTER_BOUND('',#1345,.T.);
#892=FACE_OUTER_BOUND('',#1346,.T.);
#893=FACE_OUTER_BOUND('',#1347,.T.);
#894=FACE_OUTER_BOUND('',#1348,.T.);
#895=FACE_OUTER_BOUND('',#1349,.T.);
#896=FACE_OUTER_BOUND('',#1350,.T.);
#897=FACE_OUTER_BOUND('',#1351,.T.);
#898=FACE_OUTER_BOUND('',#1352,.T.);
#899=FACE_OUTER_BOUND('',#1353,.T.);
#900=FACE_OUTER_BOUND('',#1354,.T.);
#901=FACE_OUTER_BOUND('',#1355,.T.);
#902=FACE_OUTER_BOUND('',#1356,.T.);
#903=FACE_OUTER_BOUND('',#1357,.T.);
#904=FACE_OUTER_BOUND('',#1358,.T.);
#905=FACE_OUTER_BOUND('',#1359,.T.);
#906=FACE_OUTER_BOUND('',#1360,.T.);
#907=FACE_OUTER_BOUND('',#1361,.T.);
#908=FACE_OUTER_BOUND('',#1362,.T.);
#909=FACE_OUTER_BOUND('',#1363,.T.);
#910=FACE_OUTER_BOUND('',#1364,.T.);
#911=FACE_OUTER_BOUND('',#1365,.T.);
#912=FACE_OUTER_BOUND('',#1366,.T.);
#913=FACE_OUTER_BOUND('',#1367,.T.);
#914=FACE_OUTER_BOUND('',#1368,.T.);
#915=FACE_OUTER_BOUND('',#1369,.T.);
#916=FACE_OUTER_BOUND('',#1370,.T.);
#917=FACE_OUTER_BOUND('',#1371,.T.);
#918=FACE_OUTER_BOUND('',#1372,.T.);
#919=FACE_OUTER_BOUND('',#1373,.T.);
#920=FACE_OUTER_BOUND('',#1374,.T.);
#921=FACE_OUTER_BOUND('',#1375,.T.);
#922=FACE_OUTER_BOUND('',#1376,.T.);
#923=FACE_OUTER_BOUND('',#1377,.T.);
#924=FACE_OUTER_BOUND('',#1378,.T.);
#925=FACE_OUTER_BOUND('',#1379,.T.);
#926=FACE_OUTER_BOUND('',#1380,.T.);
#927=FACE_OUTER_BOUND('',#1381,.T.);
#928=FACE_OUTER_BOUND('',#1382,.T.);
#929=FACE_OUTER_BOUND('',#1383,.T.);
#930=FACE_OUTER_BOUND('',#1384,.T.);
#931=FACE_OUTER_BOUND('',#1385,.T.);
#932=FACE_OUTER_BOUND('',#1386,.T.);
#933=FACE_OUTER_BOUND('',#1387,.T.);
#934=FACE_OUTER_BOUND('',#1388,.T.);
#935=FACE_OUTER_BOUND('',#1389,.T.);
#936=FACE_OUTER_BOUND('',#1390,.T.);
#937=FACE_OUTER_BOUND('',#1391,.T.);
#938=FACE_OUTER_BOUND('',#1392,.T.);
#939=FACE_OUTER_BOUND('',#1393,.T.);
#940=FACE_OUTER_BOUND('',#1394,.T.);
#941=FACE_OUTER_BOUND('',#1395,.T.);
#942=FACE_OUTER_BOUND('',#1396,.T.);
#943=FACE_OUTER_BOUND('',#1397,.T.);
#944=FACE_OUTER_BOUND('',#1398,.T.);
#945=FACE_OUTER_BOUND('',#1399,.T.);
#946=FACE_OUTER_BOUND('',#1400,.T.);
#947=FACE_OUTER_BOUND('',#1401,.T.);
#948=FACE_OUTER_BOUND('',#1402,.T.);
#949=FACE_OUTER_BOUND('',#1403,.T.);
#950=FACE_OUTER_BOUND('',#1404,.T.);
#951=FACE_OUTER_BOUND('',#1405,.T.);
#952=FACE_OUTER_BOUND('',#1406,.T.);
#953=FACE_OUTER_BOUND('',#1407,.T.);
#954=FACE_OUTER_BOUND('',#1408,.T.);
#955=FACE_OUTER_BOUND('',#1409,.T.);
#956=FACE_OUTER_BOUND('',#1410,.T.);
#957=FACE_OUTER_BOUND('',#1411,.T.);
#958=FACE_OUTER_BOUND('',#1412,.T.);
#959=FACE_OUTER_BOUND('',#1413,.T.);
#960=FACE_OUTER_BOUND('',#1414,.T.);
#961=FACE_OUTER_BOUND('',#1415,.T.);
#962=FACE_OUTER_BOUND('',#1416,.T.);
#963=FACE_OUTER_BOUND('',#1417,.T.);
#964=FACE_OUTER_BOUND('',#1418,.T.);
#965=FACE_OUTER_BOUND('',#1419,.T.);
#966=FACE_OUTER_BOUND('',#1420,.T.);
#967=FACE_OUTER_BOUND('',#1421,.T.);
#968=FACE_OUTER_BOUND('',#1422,.T.);
#969=FACE_OUTER_BOUND('',#1423,.T.);
#970=FACE_OUTER_BOUND('',#1425,.T.);
#971=FACE_OUTER_BOUND('',#1426,.T.);
#972=FACE_OUTER_BOUND('',#1427,.T.);
#973=FACE_OUTER_BOUND('',#1428,.T.);
#974=FACE_OUTER_BOUND('',#1429,.T.);
#975=FACE_OUTER_BOUND('',#1430,.T.);
#976=FACE_OUTER_BOUND('',#1431,.T.);
#977=FACE_OUTER_BOUND('',#1432,.T.);
#978=FACE_OUTER_BOUND('',#1433,.T.);
#979=FACE_OUTER_BOUND('',#1434,.T.);
#980=FACE_OUTER_BOUND('',#1435,.T.);
#981=FACE_OUTER_BOUND('',#1436,.T.);
#982=FACE_OUTER_BOUND('',#1437,.T.);
#983=FACE_OUTER_BOUND('',#1438,.T.);
#984=FACE_OUTER_BOUND('',#1439,.T.);
#985=FACE_OUTER_BOUND('',#1440,.T.);
#986=FACE_OUTER_BOUND('',#1441,.T.);
#987=FACE_OUTER_BOUND('',#1442,.T.);
#988=FACE_OUTER_BOUND('',#1443,.T.);
#989=FACE_OUTER_BOUND('',#1444,.T.);
#990=FACE_OUTER_BOUND('',#1446,.T.);
#991=FACE_OUTER_BOUND('',#1447,.T.);
#992=FACE_OUTER_BOUND('',#1448,.T.);
#993=FACE_OUTER_BOUND('',#1449,.T.);
#994=FACE_OUTER_BOUND('',#1450,.T.);
#995=FACE_OUTER_BOUND('',#1451,.T.);
#996=FACE_OUTER_BOUND('',#1452,.T.);
#997=FACE_OUTER_BOUND('',#1453,.T.);
#998=FACE_OUTER_BOUND('',#1454,.T.);
#999=FACE_OUTER_BOUND('',#1455,.T.);
#1000=FACE_OUTER_BOUND('',#1456,.T.);
#1001=FACE_OUTER_BOUND('',#1457,.T.);
#1002=FACE_OUTER_BOUND('',#1458,.T.);
#1003=FACE_OUTER_BOUND('',#1459,.T.);
#1004=FACE_OUTER_BOUND('',#1460,.T.);
#1005=FACE_OUTER_BOUND('',#1461,.T.);
#1006=FACE_OUTER_BOUND('',#1462,.T.);
#1007=FACE_OUTER_BOUND('',#1464,.T.);
#1008=FACE_OUTER_BOUND('',#1466,.T.);
#1009=FACE_OUTER_BOUND('',#1467,.T.);
#1010=FACE_OUTER_BOUND('',#1468,.T.);
#1011=FACE_OUTER_BOUND('',#1469,.T.);
#1012=FACE_OUTER_BOUND('',#1470,.T.);
#1013=FACE_OUTER_BOUND('',#1471,.T.);
#1014=FACE_OUTER_BOUND('',#1472,.T.);
#1015=FACE_OUTER_BOUND('',#1473,.T.);
#1016=FACE_OUTER_BOUND('',#1474,.T.);
#1017=FACE_OUTER_BOUND('',#1475,.T.);
#1018=FACE_OUTER_BOUND('',#1477,.T.);
#1019=EDGE_LOOP('',(#4005,#4006,#4007,#4008));
#1020=EDGE_LOOP('',(#4009,#4010,#4011,#4012));
#1021=EDGE_LOOP('',(#4013,#4014,#4015,#4016));
#1022=EDGE_LOOP('',(#4017,#4018,#4019,#4020));
#1023=EDGE_LOOP('',(#4021,#4022,#4023,#4024));
#1024=EDGE_LOOP('',(#4025,#4026,#4027,#4028));
#1025=EDGE_LOOP('',(#4029,#4030,#4031,#4032));
#1026=EDGE_LOOP('',(#4033));
#1027=EDGE_LOOP('',(#4034));
#1028=EDGE_LOOP('',(#4035,#4036,#4037,#4038));
#1029=EDGE_LOOP('',(#4039));
#1030=EDGE_LOOP('',(#4040));
#1031=EDGE_LOOP('',(#4041,#4042,#4043,#4044));
#1032=EDGE_LOOP('',(#4045,#4046,#4047,#4048));
#1033=EDGE_LOOP('',(#4049,#4050,#4051,#4052));
#1034=EDGE_LOOP('',(#4053,#4054,#4055,#4056));
#1035=EDGE_LOOP('',(#4057,#4058,#4059,#4060));
#1036=EDGE_LOOP('',(#4061,#4062,#4063,#4064));
#1037=EDGE_LOOP('',(#4065,#4066,#4067,#4068));
#1038=EDGE_LOOP('',(#4069,#4070,#4071,#4072));
#1039=EDGE_LOOP('',(#4073));
#1040=EDGE_LOOP('',(#4074));
#1041=EDGE_LOOP('',(#4075,#4076,#4077,#4078));
#1042=EDGE_LOOP('',(#4079,#4080,#4081,#4082));
#1043=EDGE_LOOP('',(#4083));
#1044=EDGE_LOOP('',(#4084));
#1045=EDGE_LOOP('',(#4085));
#1046=EDGE_LOOP('',(#4086));
#1047=EDGE_LOOP('',(#4087));
#1048=EDGE_LOOP('',(#4088,#4089,#4090,#4091,#4092,#4093));
#1049=EDGE_LOOP('',(#4094,#4095,#4096,#4097,#4098,#4099));
#1050=EDGE_LOOP('',(#4100,#4101,#4102,#4103));
#1051=EDGE_LOOP('',(#4104));
#1052=EDGE_LOOP('',(#4105));
#1053=EDGE_LOOP('',(#4106));
#1054=EDGE_LOOP('',(#4107));
#1055=EDGE_LOOP('',(#4108));
#1056=EDGE_LOOP('',(#4109,#4110,#4111,#4112));
#1057=EDGE_LOOP('',(#4113,#4114,#4115,#4116));
#1058=EDGE_LOOP('',(#4117));
#1059=EDGE_LOOP('',(#4118));
#1060=EDGE_LOOP('',(#4119,#4120,#4121,#4122));
#1061=EDGE_LOOP('',(#4123,#4124,#4125,#4126));
#1062=EDGE_LOOP('',(#4127));
#1063=EDGE_LOOP('',(#4128));
#1064=EDGE_LOOP('',(#4129));
#1065=EDGE_LOOP('',(#4130));
#1066=EDGE_LOOP('',(#4131,#4132,#4133,#4134));
#1067=EDGE_LOOP('',(#4135,#4136,#4137,#4138));
#1068=EDGE_LOOP('',(#4139));
#1069=EDGE_LOOP('',(#4140));
#1070=EDGE_LOOP('',(#4141));
#1071=EDGE_LOOP('',(#4142));
#1072=EDGE_LOOP('',(#4143,#4144,#4145,#4146));
#1073=EDGE_LOOP('',(#4147,#4148,#4149,#4150));
#1074=EDGE_LOOP('',(#4151));
#1075=EDGE_LOOP('',(#4152));
#1076=EDGE_LOOP('',(#4153));
#1077=EDGE_LOOP('',(#4154));
#1078=EDGE_LOOP('',(#4155,#4156,#4157,#4158));
#1079=EDGE_LOOP('',(#4159,#4160,#4161,#4162));
#1080=EDGE_LOOP('',(#4163));
#1081=EDGE_LOOP('',(#4164));
#1082=EDGE_LOOP('',(#4165));
#1083=EDGE_LOOP('',(#4166));
#1084=EDGE_LOOP('',(#4167,#4168,#4169,#4170));
#1085=EDGE_LOOP('',(#4171,#4172,#4173,#4174));
#1086=EDGE_LOOP('',(#4175,#4176,#4177,#4178));
#1087=EDGE_LOOP('',(#4179,#4180,#4181,#4182));
#1088=EDGE_LOOP('',(#4183,#4184,#4185,#4186));
#1089=EDGE_LOOP('',(#4187,#4188,#4189,#4190));
#1090=EDGE_LOOP('',(#4191,#4192,#4193,#4194));
#1091=EDGE_LOOP('',(#4195,#4196,#4197,#4198));
#1092=EDGE_LOOP('',(#4199,#4200,#4201,#4202));
#1093=EDGE_LOOP('',(#4203,#4204,#4205,#4206));
#1094=EDGE_LOOP('',(#4207,#4208,#4209,#4210));
#1095=EDGE_LOOP('',(#4211,#4212,#4213,#4214));
#1096=EDGE_LOOP('',(#4215,#4216,#4217,#4218));
#1097=EDGE_LOOP('',(#4219,#4220,#4221,#4222));
#1098=EDGE_LOOP('',(#4223,#4224,#4225,#4226));
#1099=EDGE_LOOP('',(#4227,#4228,#4229,#4230));
#1100=EDGE_LOOP('',(#4231,#4232,#4233,#4234));
#1101=EDGE_LOOP('',(#4235,#4236,#4237,#4238));
#1102=EDGE_LOOP('',(#4239,#4240,#4241,#4242,#4243,#4244));
#1103=EDGE_LOOP('',(#4245,#4246,#4247,#4248,#4249,#4250));
#1104=EDGE_LOOP('',(#4251));
#1105=EDGE_LOOP('',(#4252));
#1106=EDGE_LOOP('',(#4253,#4254,#4255,#4256));
#1107=EDGE_LOOP('',(#4257,#4258,#4259,#4260));
#1108=EDGE_LOOP('',(#4261,#4262,#4263,#4264));
#1109=EDGE_LOOP('',(#4265));
#1110=EDGE_LOOP('',(#4266));
#1111=EDGE_LOOP('',(#4267,#4268,#4269,#4270));
#1112=EDGE_LOOP('',(#4271,#4272,#4273,#4274));
#1113=EDGE_LOOP('',(#4275,#4276,#4277,#4278));
#1114=EDGE_LOOP('',(#4279,#4280,#4281,#4282));
#1115=EDGE_LOOP('',(#4283,#4284));
#1116=EDGE_LOOP('',(#4285));
#1117=EDGE_LOOP('',(#4286));
#1118=EDGE_LOOP('',(#4287,#4288,#4289,#4290));
#1119=EDGE_LOOP('',(#4291,#4292,#4293,#4294));
#1120=EDGE_LOOP('',(#4295));
#1121=EDGE_LOOP('',(#4296));
#1122=EDGE_LOOP('',(#4297));
#1123=EDGE_LOOP('',(#4298));
#1124=EDGE_LOOP('',(#4299,#4300,#4301,#4302));
#1125=EDGE_LOOP('',(#4303,#4304,#4305,#4306));
#1126=EDGE_LOOP('',(#4307,#4308,#4309,#4310));
#1127=EDGE_LOOP('',(#4311,#4312,#4313,#4314));
#1128=EDGE_LOOP('',(#4315,#4316,#4317,#4318));
#1129=EDGE_LOOP('',(#4319,#4320,#4321,#4322));
#1130=EDGE_LOOP('',(#4323,#4324,#4325,#4326));
#1131=EDGE_LOOP('',(#4327,#4328,#4329,#4330));
#1132=EDGE_LOOP('',(#4331,#4332,#4333,#4334));
#1133=EDGE_LOOP('',(#4335,#4336,#4337,#4338));
#1134=EDGE_LOOP('',(#4339,#4340,#4341,#4342));
#1135=EDGE_LOOP('',(#4343,#4344,#4345,#4346));
#1136=EDGE_LOOP('',(#4347,#4348,#4349,#4350,#4351,#4352,#4353,#4354));
#1137=EDGE_LOOP('',(#4355));
#1138=EDGE_LOOP('',(#4356));
#1139=EDGE_LOOP('',(#4357));
#1140=EDGE_LOOP('',(#4358));
#1141=EDGE_LOOP('',(#4359));
#1142=EDGE_LOOP('',(#4360,#4361,#4362,#4363,#4364,#4365,#4366,#4367));
#1143=EDGE_LOOP('',(#4368));
#1144=EDGE_LOOP('',(#4369));
#1145=EDGE_LOOP('',(#4370));
#1146=EDGE_LOOP('',(#4371));
#1147=EDGE_LOOP('',(#4372));
#1148=EDGE_LOOP('',(#4373,#4374,#4375,#4376));
#1149=EDGE_LOOP('',(#4377));
#1150=EDGE_LOOP('',(#4378));
#1151=EDGE_LOOP('',(#4379,#4380));
#1152=EDGE_LOOP('',(#4381));
#1153=EDGE_LOOP('',(#4382));
#1154=EDGE_LOOP('',(#4383));
#1155=EDGE_LOOP('',(#4384));
#1156=EDGE_LOOP('',(#4385,#4386,#4387,#4388,#4389,#4390));
#1157=EDGE_LOOP('',(#4391,#4392,#4393,#4394,#4395,#4396));
#1158=EDGE_LOOP('',(#4397,#4398,#4399,#4400));
#1159=EDGE_LOOP('',(#4401,#4402,#4403));
#1160=EDGE_LOOP('',(#4404,#4405,#4406));
#1161=EDGE_LOOP('',(#4407,#4408,#4409));
#1162=EDGE_LOOP('',(#4410,#4411,#4412));
#1163=EDGE_LOOP('',(#4413,#4414,#4415));
#1164=EDGE_LOOP('',(#4416,#4417,#4418));
#1165=EDGE_LOOP('',(#4419,#4420,#4421,#4422,#4423,#4424));
#1166=EDGE_LOOP('',(#4425,#4426,#4427,#4428,#4429,#4430));
#1167=EDGE_LOOP('',(#4431,#4432,#4433,#4434,#4435,#4436));
#1168=EDGE_LOOP('',(#4437,#4438,#4439,#4440,#4441,#4442));
#1169=EDGE_LOOP('',(#4443));
#1170=EDGE_LOOP('',(#4444));
#1171=EDGE_LOOP('',(#4445));
#1172=EDGE_LOOP('',(#4446));
#1173=EDGE_LOOP('',(#4447,#4448,#4449,#4450));
#1174=EDGE_LOOP('',(#4451));
#1175=EDGE_LOOP('',(#4452));
#1176=EDGE_LOOP('',(#4453,#4454,#4455,#4456));
#1177=EDGE_LOOP('',(#4457));
#1178=EDGE_LOOP('',(#4458));
#1179=EDGE_LOOP('',(#4459));
#1180=EDGE_LOOP('',(#4460));
#1181=EDGE_LOOP('',(#4461));
#1182=EDGE_LOOP('',(#4462));
#1183=EDGE_LOOP('',(#4463));
#1184=EDGE_LOOP('',(#4464,#4465,#4466,#4467));
#1185=EDGE_LOOP('',(#4468,#4469,#4470,#4471));
#1186=EDGE_LOOP('',(#4472,#4473,#4474,#4475));
#1187=EDGE_LOOP('',(#4476));
#1188=EDGE_LOOP('',(#4477));
#1189=EDGE_LOOP('',(#4478,#4479,#4480,#4481));
#1190=EDGE_LOOP('',(#4482,#4483,#4484,#4485));
#1191=EDGE_LOOP('',(#4486,#4487,#4488,#4489));
#1192=EDGE_LOOP('',(#4490));
#1193=EDGE_LOOP('',(#4491,#4492,#4493,#4494));
#1194=EDGE_LOOP('',(#4495,#4496,#4497,#4498));
#1195=EDGE_LOOP('',(#4499,#4500,#4501,#4502));
#1196=EDGE_LOOP('',(#4503,#4504,#4505,#4506));
#1197=EDGE_LOOP('',(#4507,#4508,#4509,#4510));
#1198=EDGE_LOOP('',(#4511,#4512,#4513,#4514));
#1199=EDGE_LOOP('',(#4515,#4516,#4517,#4518,#4519,#4520));
#1200=EDGE_LOOP('',(#4521,#4522,#4523,#4524,#4525,#4526));
#1201=EDGE_LOOP('',(#4527,#4528,#4529,#4530));
#1202=EDGE_LOOP('',(#4531,#4532,#4533,#4534));
#1203=EDGE_LOOP('',(#4535,#4536,#4537,#4538));
#1204=EDGE_LOOP('',(#4539,#4540,#4541,#4542));
#1205=EDGE_LOOP('',(#4543,#4544,#4545,#4546));
#1206=EDGE_LOOP('',(#4547,#4548,#4549,#4550));
#1207=EDGE_LOOP('',(#4551));
#1208=EDGE_LOOP('',(#4552,#4553,#4554,#4555));
#1209=EDGE_LOOP('',(#4556,#4557,#4558,#4559));
#1210=EDGE_LOOP('',(#4560,#4561,#4562,#4563));
#1211=EDGE_LOOP('',(#4564,#4565,#4566,#4567));
#1212=EDGE_LOOP('',(#4568,#4569,#4570,#4571));
#1213=EDGE_LOOP('',(#4572,#4573,#4574,#4575));
#1214=EDGE_LOOP('',(#4576));
#1215=EDGE_LOOP('',(#4577,#4578,#4579,#4580));
#1216=EDGE_LOOP('',(#4581,#4582,#4583,#4584));
#1217=EDGE_LOOP('',(#4585));
#1218=EDGE_LOOP('',(#4586));
#1219=EDGE_LOOP('',(#4587,#4588,#4589,#4590));
#1220=EDGE_LOOP('',(#4591,#4592,#4593,#4594));
#1221=EDGE_LOOP('',(#4595));
#1222=EDGE_LOOP('',(#4596));
#1223=EDGE_LOOP('',(#4597));
#1224=EDGE_LOOP('',(#4598));
#1225=EDGE_LOOP('',(#4599,#4600,#4601,#4602));
#1226=EDGE_LOOP('',(#4603,#4604,#4605,#4606));
#1227=EDGE_LOOP('',(#4607));
#1228=EDGE_LOOP('',(#4608));
#1229=EDGE_LOOP('',(#4609));
#1230=EDGE_LOOP('',(#4610));
#1231=EDGE_LOOP('',(#4611,#4612,#4613,#4614));
#1232=EDGE_LOOP('',(#4615,#4616,#4617,#4618));
#1233=EDGE_LOOP('',(#4619));
#1234=EDGE_LOOP('',(#4620));
#1235=EDGE_LOOP('',(#4621));
#1236=EDGE_LOOP('',(#4622));
#1237=EDGE_LOOP('',(#4623,#4624,#4625,#4626));
#1238=EDGE_LOOP('',(#4627,#4628,#4629,#4630));
#1239=EDGE_LOOP('',(#4631));
#1240=EDGE_LOOP('',(#4632));
#1241=EDGE_LOOP('',(#4633));
#1242=EDGE_LOOP('',(#4634));
#1243=EDGE_LOOP('',(#4635,#4636));
#1244=EDGE_LOOP('',(#4637,#4638,#4639,#4640,#4641,#4642,#4643,#4644,#4645));
#1245=EDGE_LOOP('',(#4646,#4647,#4648));
#1246=EDGE_LOOP('',(#4649,#4650,#4651,#4652));
#1247=EDGE_LOOP('',(#4653,#4654,#4655,#4656));
#1248=EDGE_LOOP('',(#4657,#4658,#4659,#4660));
#1249=EDGE_LOOP('',(#4661,#4662));
#1250=EDGE_LOOP('',(#4663));
#1251=EDGE_LOOP('',(#4664));
#1252=EDGE_LOOP('',(#4665));
#1253=EDGE_LOOP('',(#4666));
#1254=EDGE_LOOP('',(#4667,#4668));
#1255=EDGE_LOOP('',(#4669,#4670,#4671,#4672,#4673,#4674,#4675,#4676,#4677));
#1256=EDGE_LOOP('',(#4678,#4679,#4680));
#1257=EDGE_LOOP('',(#4681,#4682,#4683,#4684));
#1258=EDGE_LOOP('',(#4685,#4686,#4687,#4688));
#1259=EDGE_LOOP('',(#4689,#4690,#4691,#4692));
#1260=EDGE_LOOP('',(#4693,#4694));
#1261=EDGE_LOOP('',(#4695));
#1262=EDGE_LOOP('',(#4696));
#1263=EDGE_LOOP('',(#4697));
#1264=EDGE_LOOP('',(#4698));
#1265=EDGE_LOOP('',(#4699,#4700,#4701,#4702));
#1266=EDGE_LOOP('',(#4703,#4704,#4705,#4706));
#1267=EDGE_LOOP('',(#4707,#4708,#4709,#4710));
#1268=EDGE_LOOP('',(#4711));
#1269=EDGE_LOOP('',(#4712));
#1270=EDGE_LOOP('',(#4713));
#1271=EDGE_LOOP('',(#4714));
#1272=EDGE_LOOP('',(#4715));
#1273=EDGE_LOOP('',(#4716));
#1274=EDGE_LOOP('',(#4717));
#1275=EDGE_LOOP('',(#4718,#4719,#4720,#4721));
#1276=EDGE_LOOP('',(#4722,#4723,#4724,#4725));
#1277=EDGE_LOOP('',(#4726,#4727,#4728,#4729));
#1278=EDGE_LOOP('',(#4730,#4731,#4732,#4733));
#1279=EDGE_LOOP('',(#4734,#4735,#4736,#4737));
#1280=EDGE_LOOP('',(#4738,#4739,#4740,#4741));
#1281=EDGE_LOOP('',(#4742,#4743,#4744,#4745));
#1282=EDGE_LOOP('',(#4746,#4747,#4748,#4749));
#1283=EDGE_LOOP('',(#4750));
#1284=EDGE_LOOP('',(#4751));
#1285=EDGE_LOOP('',(#4752));
#1286=EDGE_LOOP('',(#4753));
#1287=EDGE_LOOP('',(#4754));
#1288=EDGE_LOOP('',(#4755));
#1289=EDGE_LOOP('',(#4756));
#1290=EDGE_LOOP('',(#4757));
#1291=EDGE_LOOP('',(#4758,#4759,#4760,#4761));
#1292=EDGE_LOOP('',(#4762,#4763,#4764,#4765));
#1293=EDGE_LOOP('',(#4766));
#1294=EDGE_LOOP('',(#4767,#4768,#4769,#4770));
#1295=EDGE_LOOP('',(#4771,#4772,#4773,#4774));
#1296=EDGE_LOOP('',(#4775,#4776,#4777,#4778));
#1297=EDGE_LOOP('',(#4779));
#1298=EDGE_LOOP('',(#4780));
#1299=EDGE_LOOP('',(#4781));
#1300=EDGE_LOOP('',(#4782));
#1301=EDGE_LOOP('',(#4783,#4784,#4785,#4786));
#1302=EDGE_LOOP('',(#4787,#4788,#4789,#4790));
#1303=EDGE_LOOP('',(#4791));
#1304=EDGE_LOOP('',(#4792,#4793,#4794,#4795));
#1305=EDGE_LOOP('',(#4796));
#1306=EDGE_LOOP('',(#4797,#4798,#4799,#4800));
#1307=EDGE_LOOP('',(#4801,#4802,#4803,#4804));
#1308=EDGE_LOOP('',(#4805,#4806));
#1309=EDGE_LOOP('',(#4807,#4808));
#1310=EDGE_LOOP('',(#4809,#4810));
#1311=EDGE_LOOP('',(#4811,#4812,#4813,#4814,#4815,#4816,#4817));
#1312=EDGE_LOOP('',(#4818,#4819,#4820,#4821,#4822,#4823,#4824));
#1313=EDGE_LOOP('',(#4825,#4826,#4827,#4828,#4829,#4830,#4831,#4832,#4833));
#1314=EDGE_LOOP('',(#4834,#4835,#4836));
#1315=EDGE_LOOP('',(#4837,#4838,#4839));
#1316=EDGE_LOOP('',(#4840,#4841,#4842));
#1317=EDGE_LOOP('',(#4843,#4844,#4845,#4846,#4847,#4848));
#1318=EDGE_LOOP('',(#4849,#4850,#4851,#4852,#4853,#4854,#4855));
#1319=EDGE_LOOP('',(#4856));
#1320=EDGE_LOOP('',(#4857,#4858,#4859,#4860));
#1321=EDGE_LOOP('',(#4861));
#1322=EDGE_LOOP('',(#4862,#4863,#4864,#4865,#4866,#4867,#4868,#4869,#4870,
#4871,#4872,#4873,#4874,#4875,#4876,#4877,#4878,#4879,#4880,#4881,#4882,
#4883,#4884,#4885,#4886,#4887,#4888,#4889,#4890,#4891,#4892,#4893,#4894,
#4895,#4896,#4897,#4898,#4899,#4900,#4901,#4902,#4903,#4904,#4905,#4906,
#4907,#4908,#4909,#4910,#4911,#4912,#4913,#4914,#4915,#4916,#4917,#4918,
#4919,#4920,#4921,#4922,#4923,#4924,#4925,#4926,#4927,#4928,#4929,#4930,
#4931,#4932,#4933,#4934,#4935,#4936,#4937,#4938,#4939,#4940,#4941));
#1323=EDGE_LOOP('',(#4942,#4943,#4944,#4945));
#1324=EDGE_LOOP('',(#4946));
#1325=EDGE_LOOP('',(#4947));
#1326=EDGE_LOOP('',(#4948));
#1327=EDGE_LOOP('',(#4949,#4950,#4951,#4952,#4953,#4954,#4955,#4956,#4957,
#4958,#4959,#4960,#4961,#4962,#4963,#4964,#4965,#4966,#4967,#4968,#4969,
#4970,#4971,#4972,#4973,#4974,#4975,#4976,#4977,#4978,#4979,#4980,#4981,
#4982,#4983,#4984,#4985,#4986,#4987,#4988,#4989,#4990,#4991,#4992,#4993,
#4994,#4995,#4996,#4997,#4998,#4999,#5000,#5001,#5002,#5003,#5004,#5005,
#5006,#5007,#5008,#5009,#5010,#5011,#5012,#5013,#5014,#5015,#5016,#5017,
#5018,#5019,#5020,#5021,#5022,#5023,#5024,#5025,#5026,#5027,#5028));
#1328=EDGE_LOOP('',(#5029,#5030,#5031,#5032));
#1329=EDGE_LOOP('',(#5033,#5034,#5035,#5036));
#1330=EDGE_LOOP('',(#5037,#5038,#5039,#5040));
#1331=EDGE_LOOP('',(#5041,#5042,#5043,#5044));
#1332=EDGE_LOOP('',(#5045,#5046,#5047,#5048));
#1333=EDGE_LOOP('',(#5049,#5050,#5051,#5052));
#1334=EDGE_LOOP('',(#5053,#5054,#5055,#5056));
#1335=EDGE_LOOP('',(#5057,#5058,#5059,#5060));
#1336=EDGE_LOOP('',(#5061,#5062,#5063,#5064));
#1337=EDGE_LOOP('',(#5065,#5066,#5067,#5068));
#1338=EDGE_LOOP('',(#5069,#5070,#5071,#5072));
#1339=EDGE_LOOP('',(#5073,#5074,#5075,#5076));
#1340=EDGE_LOOP('',(#5077,#5078,#5079,#5080));
#1341=EDGE_LOOP('',(#5081,#5082,#5083,#5084));
#1342=EDGE_LOOP('',(#5085,#5086,#5087,#5088));
#1343=EDGE_LOOP('',(#5089,#5090,#5091,#5092));
#1344=EDGE_LOOP('',(#5093,#5094,#5095,#5096));
#1345=EDGE_LOOP('',(#5097,#5098,#5099,#5100));
#1346=EDGE_LOOP('',(#5101,#5102,#5103,#5104));
#1347=EDGE_LOOP('',(#5105,#5106,#5107,#5108));
#1348=EDGE_LOOP('',(#5109,#5110,#5111,#5112));
#1349=EDGE_LOOP('',(#5113,#5114,#5115,#5116));
#1350=EDGE_LOOP('',(#5117,#5118,#5119,#5120));
#1351=EDGE_LOOP('',(#5121,#5122,#5123,#5124));
#1352=EDGE_LOOP('',(#5125,#5126,#5127,#5128));
#1353=EDGE_LOOP('',(#5129,#5130,#5131,#5132));
#1354=EDGE_LOOP('',(#5133,#5134,#5135,#5136));
#1355=EDGE_LOOP('',(#5137,#5138,#5139,#5140));
#1356=EDGE_LOOP('',(#5141,#5142,#5143,#5144));
#1357=EDGE_LOOP('',(#5145,#5146,#5147,#5148));
#1358=EDGE_LOOP('',(#5149,#5150,#5151,#5152));
#1359=EDGE_LOOP('',(#5153,#5154,#5155,#5156));
#1360=EDGE_LOOP('',(#5157,#5158,#5159,#5160));
#1361=EDGE_LOOP('',(#5161,#5162,#5163,#5164));
#1362=EDGE_LOOP('',(#5165,#5166,#5167,#5168));
#1363=EDGE_LOOP('',(#5169,#5170,#5171,#5172));
#1364=EDGE_LOOP('',(#5173,#5174,#5175,#5176));
#1365=EDGE_LOOP('',(#5177,#5178,#5179,#5180));
#1366=EDGE_LOOP('',(#5181,#5182,#5183,#5184));
#1367=EDGE_LOOP('',(#5185,#5186,#5187,#5188));
#1368=EDGE_LOOP('',(#5189,#5190,#5191,#5192));
#1369=EDGE_LOOP('',(#5193,#5194,#5195,#5196));
#1370=EDGE_LOOP('',(#5197,#5198,#5199,#5200));
#1371=EDGE_LOOP('',(#5201,#5202,#5203,#5204));
#1372=EDGE_LOOP('',(#5205,#5206,#5207,#5208));
#1373=EDGE_LOOP('',(#5209,#5210,#5211,#5212));
#1374=EDGE_LOOP('',(#5213,#5214,#5215,#5216));
#1375=EDGE_LOOP('',(#5217,#5218,#5219,#5220));
#1376=EDGE_LOOP('',(#5221,#5222,#5223,#5224));
#1377=EDGE_LOOP('',(#5225,#5226,#5227,#5228));
#1378=EDGE_LOOP('',(#5229,#5230,#5231,#5232));
#1379=EDGE_LOOP('',(#5233,#5234,#5235,#5236));
#1380=EDGE_LOOP('',(#5237,#5238,#5239,#5240));
#1381=EDGE_LOOP('',(#5241,#5242,#5243,#5244));
#1382=EDGE_LOOP('',(#5245,#5246,#5247,#5248));
#1383=EDGE_LOOP('',(#5249,#5250,#5251,#5252));
#1384=EDGE_LOOP('',(#5253,#5254,#5255,#5256));
#1385=EDGE_LOOP('',(#5257,#5258,#5259,#5260));
#1386=EDGE_LOOP('',(#5261,#5262,#5263,#5264));
#1387=EDGE_LOOP('',(#5265,#5266,#5267,#5268));
#1388=EDGE_LOOP('',(#5269,#5270,#5271,#5272));
#1389=EDGE_LOOP('',(#5273,#5274,#5275,#5276));
#1390=EDGE_LOOP('',(#5277,#5278,#5279,#5280));
#1391=EDGE_LOOP('',(#5281,#5282,#5283,#5284));
#1392=EDGE_LOOP('',(#5285,#5286,#5287,#5288));
#1393=EDGE_LOOP('',(#5289,#5290,#5291,#5292));
#1394=EDGE_LOOP('',(#5293,#5294,#5295,#5296));
#1395=EDGE_LOOP('',(#5297,#5298,#5299,#5300));
#1396=EDGE_LOOP('',(#5301,#5302,#5303,#5304));
#1397=EDGE_LOOP('',(#5305,#5306,#5307,#5308));
#1398=EDGE_LOOP('',(#5309,#5310,#5311,#5312));
#1399=EDGE_LOOP('',(#5313,#5314,#5315,#5316));
#1400=EDGE_LOOP('',(#5317,#5318,#5319,#5320));
#1401=EDGE_LOOP('',(#5321,#5322,#5323,#5324));
#1402=EDGE_LOOP('',(#5325,#5326,#5327,#5328));
#1403=EDGE_LOOP('',(#5329,#5330,#5331,#5332));
#1404=EDGE_LOOP('',(#5333,#5334,#5335,#5336));
#1405=EDGE_LOOP('',(#5337,#5338,#5339,#5340));
#1406=EDGE_LOOP('',(#5341,#5342,#5343,#5344));
#1407=EDGE_LOOP('',(#5345,#5346,#5347,#5348));
#1408=EDGE_LOOP('',(#5349,#5350,#5351,#5352));
#1409=EDGE_LOOP('',(#5353,#5354,#5355,#5356,#5357,#5358,#5359,#5360));
#1410=EDGE_LOOP('',(#5361,#5362,#5363,#5364));
#1411=EDGE_LOOP('',(#5365,#5366,#5367,#5368));
#1412=EDGE_LOOP('',(#5369,#5370,#5371,#5372));
#1413=EDGE_LOOP('',(#5373,#5374,#5375,#5376));
#1414=EDGE_LOOP('',(#5377,#5378,#5379,#5380,#5381,#5382,#5383,#5384));
#1415=EDGE_LOOP('',(#5385,#5386,#5387,#5388));
#1416=EDGE_LOOP('',(#5389,#5390,#5391,#5392));
#1417=EDGE_LOOP('',(#5393,#5394,#5395,#5396));
#1418=EDGE_LOOP('',(#5397,#5398,#5399,#5400));
#1419=EDGE_LOOP('',(#5401));
#1420=EDGE_LOOP('',(#5402,#5403,#5404,#5405));
#1421=EDGE_LOOP('',(#5406,#5407,#5408,#5409));
#1422=EDGE_LOOP('',(#5410,#5411,#5412,#5413));
#1423=EDGE_LOOP('',(#5414));
#1424=EDGE_LOOP('',(#5415));
#1425=EDGE_LOOP('',(#5416,#5417,#5418,#5419));
#1426=EDGE_LOOP('',(#5420,#5421,#5422,#5423));
#1427=EDGE_LOOP('',(#5424,#5425,#5426,#5427));
#1428=EDGE_LOOP('',(#5428));
#1429=EDGE_LOOP('',(#5429,#5430,#5431,#5432));
#1430=EDGE_LOOP('',(#5433,#5434,#5435,#5436));
#1431=EDGE_LOOP('',(#5437,#5438,#5439,#5440));
#1432=EDGE_LOOP('',(#5441,#5442,#5443,#5444));
#1433=EDGE_LOOP('',(#5445,#5446,#5447,#5448));
#1434=EDGE_LOOP('',(#5449,#5450,#5451,#5452));
#1435=EDGE_LOOP('',(#5453,#5454,#5455,#5456,#5457,#5458));
#1436=EDGE_LOOP('',(#5459,#5460,#5461,#5462,#5463,#5464));
#1437=EDGE_LOOP('',(#5465,#5466,#5467,#5468));
#1438=EDGE_LOOP('',(#5469,#5470,#5471,#5472));
#1439=EDGE_LOOP('',(#5473,#5474,#5475,#5476));
#1440=EDGE_LOOP('',(#5477,#5478,#5479,#5480));
#1441=EDGE_LOOP('',(#5481,#5482,#5483,#5484));
#1442=EDGE_LOOP('',(#5485,#5486,#5487,#5488));
#1443=EDGE_LOOP('',(#5489,#5490,#5491,#5492,#5493,#5494));
#1444=EDGE_LOOP('',(#5495));
#1445=EDGE_LOOP('',(#5496,#5497,#5498,#5499,#5500,#5501));
#1446=EDGE_LOOP('',(#5502,#5503,#5504,#5505));
#1447=EDGE_LOOP('',(#5506,#5507,#5508,#5509));
#1448=EDGE_LOOP('',(#5510,#5511,#5512,#5513));
#1449=EDGE_LOOP('',(#5514));
#1450=EDGE_LOOP('',(#5515,#5516,#5517,#5518,#5519,#5520,#5521,#5522));
#1451=EDGE_LOOP('',(#5523,#5524,#5525,#5526));
#1452=EDGE_LOOP('',(#5527,#5528,#5529,#5530));
#1453=EDGE_LOOP('',(#5531,#5532,#5533,#5534));
#1454=EDGE_LOOP('',(#5535,#5536,#5537,#5538));
#1455=EDGE_LOOP('',(#5539,#5540,#5541,#5542,#5543,#5544,#5545,#5546));
#1456=EDGE_LOOP('',(#5547,#5548,#5549,#5550));
#1457=EDGE_LOOP('',(#5551,#5552,#5553,#5554));
#1458=EDGE_LOOP('',(#5555,#5556,#5557,#5558));
#1459=EDGE_LOOP('',(#5559,#5560,#5561,#5562));
#1460=EDGE_LOOP('',(#5563,#5564,#5565,#5566));
#1461=EDGE_LOOP('',(#5567,#5568,#5569,#5570));
#1462=EDGE_LOOP('',(#5571));
#1463=EDGE_LOOP('',(#5572));
#1464=EDGE_LOOP('',(#5573));
#1465=EDGE_LOOP('',(#5574));
#1466=EDGE_LOOP('',(#5575,#5576,#5577,#5578,#5579,#5580,#5581,#5582,#5583));
#1467=EDGE_LOOP('',(#5584,#5585,#5586,#5587,#5588,#5589,#5590,#5591,#5592));
#1468=EDGE_LOOP('',(#5593,#5594,#5595,#5596));
#1469=EDGE_LOOP('',(#5597,#5598,#5599,#5600));
#1470=EDGE_LOOP('',(#5601,#5602,#5603,#5604));
#1471=EDGE_LOOP('',(#5605,#5606,#5607,#5608));
#1472=EDGE_LOOP('',(#5609,#5610,#5611,#5612));
#1473=EDGE_LOOP('',(#5613,#5614,#5615,#5616));
#1474=EDGE_LOOP('',(#5617,#5618,#5619,#5620));
#1475=EDGE_LOOP('',(#5621));
#1476=EDGE_LOOP('',(#5622));
#1477=EDGE_LOOP('',(#5623));
#1478=EDGE_LOOP('',(#5624));
#1479=LINE('',#9135,#1901);
#1480=LINE('',#9141,#1902);
#1481=LINE('',#9146,#1903);
#1482=LINE('',#9148,#1904);
#1483=LINE('',#9150,#1905);
#1484=LINE('',#9151,#1906);
#1485=LINE('',#9154,#1907);
#1486=LINE('',#9156,#1908);
#1487=LINE('',#9157,#1909);
#1488=LINE('',#9160,#1910);
#1489=LINE('',#9162,#1911);
#1490=LINE('',#9163,#1912);
#1491=LINE('',#9165,#1913);
#1492=LINE('',#9166,#1914);
#1493=LINE('',#9174,#1915);
#1494=LINE('',#9180,#1916);
#1495=LINE('',#9186,#1917);
#1496=LINE('',#9192,#1918);
#1497=LINE('',#9198,#1919);
#1498=LINE('',#9204,#1920);
#1499=LINE('',#9210,#1921);
#1500=LINE('',#9215,#1922);
#1501=LINE('',#9217,#1923);
#1502=LINE('',#9219,#1924);
#1503=LINE('',#9220,#1925);
#1504=LINE('',#9223,#1926);
#1505=LINE('',#9225,#1927);
#1506=LINE('',#9226,#1928);
#1507=LINE('',#9230,#1929);
#1508=LINE('',#9232,#1930);
#1509=LINE('',#9234,#1931);
#1510=LINE('',#9235,#1932);
#1511=LINE('',#9238,#1933);
#1512=LINE('',#9239,#1934);
#1513=LINE('',#9240,#1935);
#1514=LINE('',#9243,#1936);
#1515=LINE('',#9244,#1937);
#1516=LINE('',#9245,#1938);
#1517=LINE('',#9247,#1939);
#1518=LINE('',#9255,#1940);
#1519=LINE('',#9261,#1941);
#1520=LINE('',#9270,#1942);
#1521=LINE('',#9276,#1943);
#1522=LINE('',#9285,#1944);
#1523=LINE('',#9291,#1945);
#1524=LINE('',#9300,#1946);
#1525=LINE('',#9306,#1947);
#1526=LINE('',#9314,#1948);
#1527=LINE('',#9316,#1949);
#1528=LINE('',#9318,#1950);
#1529=LINE('',#9319,#1951);
#1530=LINE('',#9322,#1952);
#1531=LINE('',#9324,#1953);
#1532=LINE('',#9325,#1954);
#1533=LINE('',#9328,#1955);
#1534=LINE('',#9330,#1956);
#1535=LINE('',#9331,#1957);
#1536=LINE('',#9333,#1958);
#1537=LINE('',#9334,#1959);
#1538=LINE('',#9341,#1960);
#1539=LINE('',#9343,#1961);
#1540=LINE('',#9345,#1962);
#1541=LINE('',#9346,#1963);
#1542=LINE('',#9349,#1964);
#1543=LINE('',#9351,#1965);
#1544=LINE('',#9352,#1966);
#1545=LINE('',#9355,#1967);
#1546=LINE('',#9357,#1968);
#1547=LINE('',#9358,#1969);
#1548=LINE('',#9360,#1970);
#1549=LINE('',#9361,#1971);
#1550=LINE('',#9368,#1972);
#1551=LINE('',#9370,#1973);
#1552=LINE('',#9372,#1974);
#1553=LINE('',#9373,#1975);
#1554=LINE('',#9376,#1976);
#1555=LINE('',#9378,#1977);
#1556=LINE('',#9379,#1978);
#1557=LINE('',#9382,#1979);
#1558=LINE('',#9384,#1980);
#1559=LINE('',#9385,#1981);
#1560=LINE('',#9388,#1982);
#1561=LINE('',#9390,#1983);
#1562=LINE('',#9391,#1984);
#1563=LINE('',#9394,#1985);
#1564=LINE('',#9396,#1986);
#1565=LINE('',#9397,#1987);
#1566=LINE('',#9399,#1988);
#1567=LINE('',#9400,#1989);
#1568=LINE('',#9412,#1990);
#1569=LINE('',#9416,#1991);
#1570=LINE('',#9420,#1992);
#1571=LINE('',#9427,#1993);
#1572=LINE('',#9429,#1994);
#1573=LINE('',#9436,#1995);
#1574=LINE('',#9442,#1996);
#1575=LINE('',#9452,#1997);
#1576=LINE('',#9458,#1998);
#1577=LINE('',#9466,#1999);
#1578=LINE('',#9472,#2000);
#1579=LINE('',#9478,#2001);
#1580=LINE('',#9484,#2002);
#1581=LINE('',#9489,#2003);
#1582=LINE('',#9491,#2004);
#1583=LINE('',#9493,#2005);
#1584=LINE('',#9494,#2006);
#1585=LINE('',#9497,#2007);
#1586=LINE('',#9499,#2008);
#1587=LINE('',#9500,#2009);
#1588=LINE('',#9503,#2010);
#1589=LINE('',#9505,#2011);
#1590=LINE('',#9506,#2012);
#1591=LINE('',#9509,#2013);
#1592=LINE('',#9511,#2014);
#1593=LINE('',#9512,#2015);
#1594=LINE('',#9515,#2016);
#1595=LINE('',#9517,#2017);
#1596=LINE('',#9518,#2018);
#1597=LINE('',#9521,#2019);
#1598=LINE('',#9523,#2020);
#1599=LINE('',#9524,#2021);
#1600=LINE('',#9527,#2022);
#1601=LINE('',#9529,#2023);
#1602=LINE('',#9530,#2024);
#1603=LINE('',#9532,#2025);
#1604=LINE('',#9533,#2026);
#1605=LINE('',#9541,#2027);
#1606=LINE('',#9596,#2028);
#1607=LINE('',#9668,#2029);
#1608=LINE('',#9713,#2030);
#1609=LINE('',#9881,#2031);
#1610=LINE('',#9952,#2032);
#1611=LINE('',#9955,#2033);
#1612=LINE('',#10026,#2034);
#1613=LINE('',#10036,#2035);
#1614=LINE('',#10041,#2036);
#1615=LINE('',#10051,#2037);
#1616=LINE('',#10055,#2038);
#1617=LINE('',#10059,#2039);
#1618=LINE('',#10066,#2040);
#1619=LINE('',#10070,#2041);
#1620=LINE('',#10074,#2042);
#1621=LINE('',#10079,#2043);
#1622=LINE('',#10081,#2044);
#1623=LINE('',#10083,#2045);
#1624=LINE('',#10084,#2046);
#1625=LINE('',#10087,#2047);
#1626=LINE('',#10089,#2048);
#1627=LINE('',#10090,#2049);
#1628=LINE('',#10093,#2050);
#1629=LINE('',#10095,#2051);
#1630=LINE('',#10096,#2052);
#1631=LINE('',#10099,#2053);
#1632=LINE('',#10101,#2054);
#1633=LINE('',#10102,#2055);
#1634=LINE('',#10105,#2056);
#1635=LINE('',#10107,#2057);
#1636=LINE('',#10108,#2058);
#1637=LINE('',#10110,#2059);
#1638=LINE('',#10111,#2060);
#1639=LINE('',#10119,#2061);
#1640=LINE('',#10121,#2062);
#1641=LINE('',#10123,#2063);
#1642=LINE('',#10124,#2064);
#1643=LINE('',#10129,#2065);
#1644=LINE('',#10130,#2066);
#1645=LINE('',#10133,#2067);
#1646=LINE('',#10135,#2068);
#1647=LINE('',#10136,#2069);
#1648=LINE('',#10138,#2070);
#1649=LINE('',#10145,#2071);
#1650=LINE('',#10151,#2072);
#1651=LINE('',#10153,#2073);
#1652=LINE('',#10155,#2074);
#1653=LINE('',#10156,#2075);
#1654=LINE('',#10161,#2076);
#1655=LINE('',#10162,#2077);
#1656=LINE('',#10165,#2078);
#1657=LINE('',#10167,#2079);
#1658=LINE('',#10168,#2080);
#1659=LINE('',#10170,#2081);
#1660=LINE('',#10177,#2082);
#1661=LINE('',#10184,#2083);
#1662=LINE('',#10191,#2084);
#1663=LINE('',#10200,#2085);
#1664=LINE('',#10206,#2086);
#1665=LINE('',#10215,#2087);
#1666=LINE('',#10221,#2088);
#1667=LINE('',#10230,#2089);
#1668=LINE('',#10236,#2090);
#1669=LINE('',#10244,#2091);
#1670=LINE('',#10265,#2092);
#1671=LINE('',#10320,#2093);
#1672=LINE('',#10325,#2094);
#1673=LINE('',#10331,#2095);
#1674=LINE('',#10339,#2096);
#1675=LINE('',#10360,#2097);
#1676=LINE('',#10415,#2098);
#1677=LINE('',#10420,#2099);
#1678=LINE('',#10426,#2100);
#1679=LINE('',#10434,#2101);
#1680=LINE('',#10436,#2102);
#1681=LINE('',#10438,#2103);
#1682=LINE('',#10439,#2104);
#1683=LINE('',#10442,#2105);
#1684=LINE('',#10444,#2106);
#1685=LINE('',#10445,#2107);
#1686=LINE('',#10448,#2108);
#1687=LINE('',#10450,#2109);
#1688=LINE('',#10451,#2110);
#1689=LINE('',#10473,#2111);
#1690=LINE('',#10477,#2112);
#1691=LINE('',#10481,#2113);
#1692=LINE('',#10485,#2114);
#1693=LINE('',#10489,#2115);
#1694=LINE('',#10493,#2116);
#1695=LINE('',#10500,#2117);
#1696=LINE('',#10503,#2118);
#1697=LINE('',#10511,#2119);
#1698=LINE('',#10517,#2120);
#1699=LINE('',#10525,#2121);
#1700=LINE('',#10527,#2122);
#1701=LINE('',#10529,#2123);
#1702=LINE('',#10530,#2124);
#1703=LINE('',#10533,#2125);
#1704=LINE('',#10535,#2126);
#1705=LINE('',#10536,#2127);
#1706=LINE('',#10541,#2128);
#1707=LINE('',#10543,#2129);
#1708=LINE('',#10544,#2130);
#1709=LINE('',#10707,#2131);
#1710=LINE('',#10710,#2132);
#1711=LINE('',#10754,#2133);
#1712=LINE('',#10756,#2134);
#1713=LINE('',#10841,#2135);
#1714=LINE('',#10843,#2136);
#1715=LINE('',#11011,#2137);
#1716=LINE('',#11177,#2138);
#1717=LINE('',#11179,#2139);
#1718=LINE('',#11180,#2140);
#1719=LINE('',#11182,#2141);
#1720=LINE('',#11184,#2142);
#1721=LINE('',#11186,#2143);
#1722=LINE('',#11188,#2144);
#1723=LINE('',#11190,#2145);
#1724=LINE('',#11192,#2146);
#1725=LINE('',#11194,#2147);
#1726=LINE('',#11196,#2148);
#1727=LINE('',#11198,#2149);
#1728=LINE('',#11200,#2150);
#1729=LINE('',#11202,#2151);
#1730=LINE('',#11204,#2152);
#1731=LINE('',#11206,#2153);
#1732=LINE('',#11208,#2154);
#1733=LINE('',#11210,#2155);
#1734=LINE('',#11212,#2156);
#1735=LINE('',#11214,#2157);
#1736=LINE('',#11216,#2158);
#1737=LINE('',#11218,#2159);
#1738=LINE('',#11220,#2160);
#1739=LINE('',#11222,#2161);
#1740=LINE('',#11224,#2162);
#1741=LINE('',#11226,#2163);
#1742=LINE('',#11228,#2164);
#1743=LINE('',#11230,#2165);
#1744=LINE('',#11232,#2166);
#1745=LINE('',#11234,#2167);
#1746=LINE('',#11236,#2168);
#1747=LINE('',#11238,#2169);
#1748=LINE('',#11240,#2170);
#1749=LINE('',#11242,#2171);
#1750=LINE('',#11244,#2172);
#1751=LINE('',#11246,#2173);
#1752=LINE('',#11248,#2174);
#1753=LINE('',#11250,#2175);
#1754=LINE('',#11252,#2176);
#1755=LINE('',#11254,#2177);
#1756=LINE('',#11256,#2178);
#1757=LINE('',#11258,#2179);
#1758=LINE('',#11260,#2180);
#1759=LINE('',#11262,#2181);
#1760=LINE('',#11264,#2182);
#1761=LINE('',#11266,#2183);
#1762=LINE('',#11268,#2184);
#1763=LINE('',#11270,#2185);
#1764=LINE('',#11272,#2186);
#1765=LINE('',#11274,#2187);
#1766=LINE('',#11276,#2188);
#1767=LINE('',#11278,#2189);
#1768=LINE('',#11280,#2190);
#1769=LINE('',#11282,#2191);
#1770=LINE('',#11284,#2192);
#1771=LINE('',#11286,#2193);
#1772=LINE('',#11288,#2194);
#1773=LINE('',#11290,#2195);
#1774=LINE('',#11292,#2196);
#1775=LINE('',#11294,#2197);
#1776=LINE('',#11296,#2198);
#1777=LINE('',#11298,#2199);
#1778=LINE('',#11300,#2200);
#1779=LINE('',#11302,#2201);
#1780=LINE('',#11304,#2202);
#1781=LINE('',#11306,#2203);
#1782=LINE('',#11308,#2204);
#1783=LINE('',#11310,#2205);
#1784=LINE('',#11312,#2206);
#1785=LINE('',#11314,#2207);
#1786=LINE('',#11316,#2208);
#1787=LINE('',#11318,#2209);
#1788=LINE('',#11320,#2210);
#1789=LINE('',#11322,#2211);
#1790=LINE('',#11324,#2212);
#1791=LINE('',#11326,#2213);
#1792=LINE('',#11328,#2214);
#1793=LINE('',#11330,#2215);
#1794=LINE('',#11332,#2216);
#1795=LINE('',#11334,#2217);
#1796=LINE('',#11336,#2218);
#1797=LINE('',#11342,#2219);
#1798=LINE('',#11344,#2220);
#1799=LINE('',#11346,#2221);
#1800=LINE('',#11348,#2222);
#1801=LINE('',#11350,#2223);
#1802=LINE('',#11352,#2224);
#1803=LINE('',#11354,#2225);
#1804=LINE('',#11355,#2226);
#1805=LINE('',#11358,#2227);
#1806=LINE('',#11360,#2228);
#1807=LINE('',#11361,#2229);
#1808=LINE('',#11364,#2230);
#1809=LINE('',#11365,#2231);
#1810=LINE('',#11368,#2232);
#1811=LINE('',#11369,#2233);
#1812=LINE('',#11372,#2234);
#1813=LINE('',#11373,#2235);
#1814=LINE('',#11376,#2236);
#1815=LINE('',#11378,#2237);
#1816=LINE('',#11380,#2238);
#1817=LINE('',#11381,#2239);
#1818=LINE('',#11383,#2240);
#1819=LINE('',#11385,#2241);
#1820=LINE('',#11387,#2242);
#1821=LINE('',#11396,#2243);
#1822=LINE('',#11400,#2244);
#1823=LINE('',#11404,#2245);
#1824=LINE('',#11411,#2246);
#1825=LINE('',#11415,#2247);
#1826=LINE('',#11419,#2248);
#1827=LINE('',#11424,#2249);
#1828=LINE('',#11426,#2250);
#1829=LINE('',#11428,#2251);
#1830=LINE('',#11429,#2252);
#1831=LINE('',#11432,#2253);
#1832=LINE('',#11434,#2254);
#1833=LINE('',#11435,#2255);
#1834=LINE('',#11438,#2256);
#1835=LINE('',#11440,#2257);
#1836=LINE('',#11441,#2258);
#1837=LINE('',#11444,#2259);
#1838=LINE('',#11446,#2260);
#1839=LINE('',#11447,#2261);
#1840=LINE('',#11450,#2262);
#1841=LINE('',#11452,#2263);
#1842=LINE('',#11453,#2264);
#1843=LINE('',#11455,#2265);
#1844=LINE('',#11456,#2266);
#1845=LINE('',#11463,#2267);
#1846=LINE('',#11465,#2268);
#1847=LINE('',#11467,#2269);
#1848=LINE('',#11468,#2270);
#1849=LINE('',#11471,#2271);
#1850=LINE('',#11473,#2272);
#1851=LINE('',#11474,#2273);
#1852=LINE('',#11477,#2274);
#1853=LINE('',#11479,#2275);
#1854=LINE('',#11480,#2276);
#1855=LINE('',#11483,#2277);
#1856=LINE('',#11485,#2278);
#1857=LINE('',#11486,#2279);
#1858=LINE('',#11489,#2280);
#1859=LINE('',#11491,#2281);
#1860=LINE('',#11492,#2282);
#1861=LINE('',#11494,#2283);
#1862=LINE('',#11495,#2284);
#1863=LINE('',#11503,#2285);
#1864=LINE('',#11507,#2286);
#1865=LINE('',#11511,#2287);
#1866=LINE('',#11517,#2288);
#1867=LINE('',#11519,#2289);
#1868=LINE('',#11521,#2290);
#1869=LINE('',#11523,#2291);
#1870=LINE('',#11525,#2292);
#1871=LINE('',#11527,#2293);
#1872=LINE('',#11529,#2294);
#1873=LINE('',#11530,#2295);
#1874=LINE('',#11533,#2296);
#1875=LINE('',#11535,#2297);
#1876=LINE('',#11536,#2298);
#1877=LINE('',#11539,#2299);
#1878=LINE('',#11540,#2300);
#1879=LINE('',#11543,#2301);
#1880=LINE('',#11544,#2302);
#1881=LINE('',#11547,#2303);
#1882=LINE('',#11548,#2304);
#1883=LINE('',#11552,#2305);
#1884=LINE('',#11553,#2306);
#1885=LINE('',#11555,#2307);
#1886=LINE('',#11556,#2308);
#1887=LINE('',#11558,#2309);
#1888=LINE('',#11560,#2310);
#1889=LINE('',#11562,#2311);
#1890=LINE('',#11569,#2312);
#1891=LINE('',#11575,#2313);
#1892=LINE('',#11591,#2314);
#1893=LINE('',#11612,#2315);
#1894=LINE('',#11637,#2316);
#1895=LINE('',#11638,#2317);
#1896=LINE('',#11640,#2318);
#1897=LINE('',#11642,#2319);
#1898=LINE('',#11647,#2320);
#1899=LINE('',#11650,#2321);
#1900=LINE('',#11652,#2322);
#1901=VECTOR('',#7218,0.25);
#1902=VECTOR('',#7225,0.25);
#1903=VECTOR('',#7230,1.);
#1904=VECTOR('',#7231,1.);
#1905=VECTOR('',#7232,1.);
#1906=VECTOR('',#7233,1.);
#1907=VECTOR('',#7236,1.);
#1908=VECTOR('',#7237,1.);
#1909=VECTOR('',#7238,1.);
#1910=VECTOR('',#7241,1.);
#1911=VECTOR('',#7242,1.);
#1912=VECTOR('',#7243,1.);
#1913=VECTOR('',#7246,1.);
#1914=VECTOR('',#7247,1.);
#1915=VECTOR('',#7258,0.33);
#1916=VECTOR('',#7265,0.33);
#1917=VECTOR('',#7272,0.44);
#1918=VECTOR('',#7279,0.44);
#1919=VECTOR('',#7286,0.44);
#1920=VECTOR('',#7293,0.44);
#1921=VECTOR('',#7300,3.1);
#1922=VECTOR('',#7305,1.);
#1923=VECTOR('',#7306,1.);
#1924=VECTOR('',#7307,1.);
#1925=VECTOR('',#7308,1.);
#1926=VECTOR('',#7311,1.);
#1927=VECTOR('',#7312,1.);
#1928=VECTOR('',#7313,1.);
#1929=VECTOR('',#7316,1.);
#1930=VECTOR('',#7317,1.);
#1931=VECTOR('',#7318,1.);
#1932=VECTOR('',#7319,1.);
#1933=VECTOR('',#7322,1.);
#1934=VECTOR('',#7323,1.);
#1935=VECTOR('',#7324,1.);
#1936=VECTOR('',#7327,1.);
#1937=VECTOR('',#7328,1.);
#1938=VECTOR('',#7329,1.);
#1939=VECTOR('',#7332,1.);
#1940=VECTOR('',#7343,0.425);
#1941=VECTOR('',#7350,0.595);
#1942=VECTOR('',#7363,0.425);
#1943=VECTOR('',#7370,0.595);
#1944=VECTOR('',#7383,0.425);
#1945=VECTOR('',#7390,0.595);
#1946=VECTOR('',#7403,0.425);
#1947=VECTOR('',#7410,0.595);
#1948=VECTOR('',#7421,1.);
#1949=VECTOR('',#7422,1.);
#1950=VECTOR('',#7423,1.);
#1951=VECTOR('',#7424,1.);
#1952=VECTOR('',#7427,1.);
#1953=VECTOR('',#7428,1.);
#1954=VECTOR('',#7429,1.);
#1955=VECTOR('',#7432,1.);
#1956=VECTOR('',#7433,1.);
#1957=VECTOR('',#7434,1.);
#1958=VECTOR('',#7437,1.);
#1959=VECTOR('',#7438,1.);
#1960=VECTOR('',#7447,1.);
#1961=VECTOR('',#7448,1.);
#1962=VECTOR('',#7449,1.);
#1963=VECTOR('',#7450,1.);
#1964=VECTOR('',#7453,1.);
#1965=VECTOR('',#7454,1.);
#1966=VECTOR('',#7455,1.);
#1967=VECTOR('',#7458,1.);
#1968=VECTOR('',#7459,1.);
#1969=VECTOR('',#7460,1.);
#1970=VECTOR('',#7463,1.);
#1971=VECTOR('',#7464,1.);
#1972=VECTOR('',#7473,1.);
#1973=VECTOR('',#7474,1.);
#1974=VECTOR('',#7475,1.);
#1975=VECTOR('',#7476,1.);
#1976=VECTOR('',#7479,1.);
#1977=VECTOR('',#7480,1.);
#1978=VECTOR('',#7481,1.);
#1979=VECTOR('',#7484,1.);
#1980=VECTOR('',#7485,1.);
#1981=VECTOR('',#7486,1.);
#1982=VECTOR('',#7489,1.);
#1983=VECTOR('',#7490,1.);
#1984=VECTOR('',#7491,1.);
#1985=VECTOR('',#7494,1.);
#1986=VECTOR('',#7495,1.);
#1987=VECTOR('',#7496,1.);
#1988=VECTOR('',#7499,1.);
#1989=VECTOR('',#7500,1.);
#1990=VECTOR('',#7517,0.475);
#1991=VECTOR('',#7522,0.5);
#1992=VECTOR('',#7527,0.485);
#1993=VECTOR('',#7536,0.31);
#1994=VECTOR('',#7539,0.3);
#1995=VECTOR('',#7548,2.05);
#1996=VECTOR('',#7555,2.05);
#1997=VECTOR('',#7566,3.);
#1998=VECTOR('',#7573,3.);
#1999=VECTOR('',#7584,0.6);
#2000=VECTOR('',#7591,0.6);
#2001=VECTOR('',#7598,0.6);
#2002=VECTOR('',#7605,0.6);
#2003=VECTOR('',#7610,1.);
#2004=VECTOR('',#7611,1.);
#2005=VECTOR('',#7612,1.);
#2006=VECTOR('',#7613,1.);
#2007=VECTOR('',#7616,1.);
#2008=VECTOR('',#7617,1.);
#2009=VECTOR('',#7618,1.);
#2010=VECTOR('',#7621,1.);
#2011=VECTOR('',#7622,1.);
#2012=VECTOR('',#7623,1.);
#2013=VECTOR('',#7626,1.);
#2014=VECTOR('',#7627,1.);
#2015=VECTOR('',#7628,1.);
#2016=VECTOR('',#7631,1.);
#2017=VECTOR('',#7632,1.);
#2018=VECTOR('',#7633,1.);
#2019=VECTOR('',#7636,1.);
#2020=VECTOR('',#7637,1.);
#2021=VECTOR('',#7638,1.);
#2022=VECTOR('',#7641,1.);
#2023=VECTOR('',#7642,1.);
#2024=VECTOR('',#7643,1.);
#2025=VECTOR('',#7646,1.);
#2026=VECTOR('',#7647,1.);
#2027=VECTOR('',#7658,1.8);
#2028=VECTOR('',#7675,0.25);
#2029=VECTOR('',#7678,0.25);
#2030=VECTOR('',#7683,1.65);
#2031=VECTOR('',#7688,0.25);
#2032=VECTOR('',#7691,0.25);
#2033=VECTOR('',#7694,0.25);
#2034=VECTOR('',#7697,0.25);
#2035=VECTOR('',#7710,1.75);
#2036=VECTOR('',#7717,1.);
#2037=VECTOR('',#7732,0.625);
#2038=VECTOR('',#7737,0.65);
#2039=VECTOR('',#7742,0.635);
#2040=VECTOR('',#7751,0.41);
#2041=VECTOR('',#7756,0.4);
#2042=VECTOR('',#7761,0.36);
#2043=VECTOR('',#7766,1.);
#2044=VECTOR('',#7767,1.);
#2045=VECTOR('',#7768,1.);
#2046=VECTOR('',#7769,1.);
#2047=VECTOR('',#7772,1.);
#2048=VECTOR('',#7773,1.);
#2049=VECTOR('',#7774,1.);
#2050=VECTOR('',#7777,1.);
#2051=VECTOR('',#7778,1.);
#2052=VECTOR('',#7779,1.);
#2053=VECTOR('',#7782,1.);
#2054=VECTOR('',#7783,1.);
#2055=VECTOR('',#7784,1.);
#2056=VECTOR('',#7787,1.);
#2057=VECTOR('',#7788,1.);
#2058=VECTOR('',#7789,1.);
#2059=VECTOR('',#7792,1.);
#2060=VECTOR('',#7793,1.);
#2061=VECTOR('',#7804,1.);
#2062=VECTOR('',#7805,1.);
#2063=VECTOR('',#7806,1.);
#2064=VECTOR('',#7807,1.);
#2065=VECTOR('',#7812,1.);
#2066=VECTOR('',#7813,1.);
#2067=VECTOR('',#7816,1.);
#2068=VECTOR('',#7817,1.);
#2069=VECTOR('',#7818,1.);
#2070=VECTOR('',#7821,1.);
#2071=VECTOR('',#7830,0.21);
#2072=VECTOR('',#7837,1.);
#2073=VECTOR('',#7838,1.);
#2074=VECTOR('',#7839,1.);
#2075=VECTOR('',#7840,1.);
#2076=VECTOR('',#7845,1.);
#2077=VECTOR('',#7846,1.);
#2078=VECTOR('',#7849,1.);
#2079=VECTOR('',#7850,1.);
#2080=VECTOR('',#7851,1.);
#2081=VECTOR('',#7854,1.);
#2082=VECTOR('',#7863,0.4);
#2083=VECTOR('',#7872,0.6);
#2084=VECTOR('',#7881,1.);
#2085=VECTOR('',#7894,0.605);
#2086=VECTOR('',#7901,0.9);
#2087=VECTOR('',#7914,0.605);
#2088=VECTOR('',#7921,0.9);
#2089=VECTOR('',#7934,0.275);
#2090=VECTOR('',#7941,1.);
#2091=VECTOR('',#7952,1.);
#2092=VECTOR('',#7959,0.21);
#2093=VECTOR('',#7964,1.);
#2094=VECTOR('',#7969,1.005);
#2095=VECTOR('',#7976,1.5);
#2096=VECTOR('',#7987,1.);
#2097=VECTOR('',#7994,0.21);
#2098=VECTOR('',#7999,1.);
#2099=VECTOR('',#8004,1.005);
#2100=VECTOR('',#8011,1.5);
#2101=VECTOR('',#8022,1.);
#2102=VECTOR('',#8023,1.);
#2103=VECTOR('',#8024,1.);
#2104=VECTOR('',#8025,1.);
#2105=VECTOR('',#8028,1.);
#2106=VECTOR('',#8029,1.);
#2107=VECTOR('',#8030,1.);
#2108=VECTOR('',#8033,1.);
#2109=VECTOR('',#8034,1.);
#2110=VECTOR('',#8035,1.);
#2111=VECTOR('',#8062,0.33);
#2112=VECTOR('',#8067,0.33);
#2113=VECTOR('',#8072,0.33);
#2114=VECTOR('',#8077,0.33);
#2115=VECTOR('',#8082,0.33);
#2116=VECTOR('',#8087,0.33);
#2117=VECTOR('',#8096,6.);
#2118=VECTOR('',#8099,1.8);
#2119=VECTOR('',#8110,0.425);
#2120=VECTOR('',#8117,1.4);
#2121=VECTOR('',#8128,1.);
#2122=VECTOR('',#8129,1.);
#2123=VECTOR('',#8130,1.);
#2124=VECTOR('',#8131,1.);
#2125=VECTOR('',#8134,1.);
#2126=VECTOR('',#8135,1.);
#2127=VECTOR('',#8136,1.);
#2128=VECTOR('',#8141,1.);
#2129=VECTOR('',#8142,1.);
#2130=VECTOR('',#8143,1.);
#2131=VECTOR('',#8156,0.125);
#2132=VECTOR('',#8159,0.125);
#2133=VECTOR('',#8164,1.);
#2134=VECTOR('',#8165,1.);
#2135=VECTOR('',#8170,0.125);
#2136=VECTOR('',#8173,0.125);
#2137=VECTOR('',#8344,1.4);
#2138=VECTOR('',#8513,1.4);
#2139=VECTOR('',#8516,1.);
#2140=VECTOR('',#8517,1.);
#2141=VECTOR('',#8520,1.);
#2142=VECTOR('',#8523,1.);
#2143=VECTOR('',#8526,1.);
#2144=VECTOR('',#8529,1.);
#2145=VECTOR('',#8532,1.);
#2146=VECTOR('',#8535,1.);
#2147=VECTOR('',#8538,1.);
#2148=VECTOR('',#8541,1.);
#2149=VECTOR('',#8544,1.);
#2150=VECTOR('',#8547,1.);
#2151=VECTOR('',#8550,1.);
#2152=VECTOR('',#8553,1.);
#2153=VECTOR('',#8556,1.);
#2154=VECTOR('',#8559,1.);
#2155=VECTOR('',#8562,1.);
#2156=VECTOR('',#8565,1.);
#2157=VECTOR('',#8568,1.);
#2158=VECTOR('',#8571,1.);
#2159=VECTOR('',#8574,1.);
#2160=VECTOR('',#8577,1.);
#2161=VECTOR('',#8580,1.);
#2162=VECTOR('',#8583,1.);
#2163=VECTOR('',#8586,1.);
#2164=VECTOR('',#8589,1.);
#2165=VECTOR('',#8592,1.);
#2166=VECTOR('',#8595,1.);
#2167=VECTOR('',#8598,1.);
#2168=VECTOR('',#8601,1.);
#2169=VECTOR('',#8604,1.);
#2170=VECTOR('',#8607,1.);
#2171=VECTOR('',#8610,1.);
#2172=VECTOR('',#8613,1.);
#2173=VECTOR('',#8616,1.);
#2174=VECTOR('',#8619,1.);
#2175=VECTOR('',#8622,1.);
#2176=VECTOR('',#8625,1.);
#2177=VECTOR('',#8628,1.);
#2178=VECTOR('',#8631,1.);
#2179=VECTOR('',#8634,1.);
#2180=VECTOR('',#8637,1.);
#2181=VECTOR('',#8640,1.);
#2182=VECTOR('',#8643,1.);
#2183=VECTOR('',#8646,1.);
#2184=VECTOR('',#8649,1.);
#2185=VECTOR('',#8652,1.);
#2186=VECTOR('',#8655,1.);
#2187=VECTOR('',#8658,1.);
#2188=VECTOR('',#8661,1.);
#2189=VECTOR('',#8664,1.);
#2190=VECTOR('',#8667,1.);
#2191=VECTOR('',#8670,1.);
#2192=VECTOR('',#8673,1.);
#2193=VECTOR('',#8676,1.);
#2194=VECTOR('',#8679,1.);
#2195=VECTOR('',#8682,1.);
#2196=VECTOR('',#8685,1.);
#2197=VECTOR('',#8688,1.);
#2198=VECTOR('',#8691,1.);
#2199=VECTOR('',#8694,1.);
#2200=VECTOR('',#8697,1.);
#2201=VECTOR('',#8700,1.);
#2202=VECTOR('',#8703,1.);
#2203=VECTOR('',#8706,1.);
#2204=VECTOR('',#8709,1.);
#2205=VECTOR('',#8712,1.);
#2206=VECTOR('',#8715,1.);
#2207=VECTOR('',#8718,1.);
#2208=VECTOR('',#8721,1.);
#2209=VECTOR('',#8724,1.);
#2210=VECTOR('',#8727,1.);
#2211=VECTOR('',#8730,1.);
#2212=VECTOR('',#8733,1.);
#2213=VECTOR('',#8736,1.);
#2214=VECTOR('',#8739,1.);
#2215=VECTOR('',#8742,1.);
#2216=VECTOR('',#8745,1.);
#2217=VECTOR('',#8748,1.);
#2218=VECTOR('',#8751,1.);
#2219=VECTOR('',#8758,1.);
#2220=VECTOR('',#8759,1.);
#2221=VECTOR('',#8760,1.);
#2222=VECTOR('',#8761,1.);
#2223=VECTOR('',#8762,1.);
#2224=VECTOR('',#8763,1.);
#2225=VECTOR('',#8764,1.);
#2226=VECTOR('',#8765,1.);
#2227=VECTOR('',#8768,1.);
#2228=VECTOR('',#8769,1.);
#2229=VECTOR('',#8770,1.);
#2230=VECTOR('',#8773,1.);
#2231=VECTOR('',#8774,1.);
#2232=VECTOR('',#8777,1.);
#2233=VECTOR('',#8778,1.);
#2234=VECTOR('',#8781,1.);
#2235=VECTOR('',#8782,1.);
#2236=VECTOR('',#8785,1.);
#2237=VECTOR('',#8786,1.);
#2238=VECTOR('',#8787,1.);
#2239=VECTOR('',#8788,1.);
#2240=VECTOR('',#8791,1.);
#2241=VECTOR('',#8794,1.);
#2242=VECTOR('',#8797,1.);
#2243=VECTOR('',#8810,0.4);
#2244=VECTOR('',#8815,0.425);
#2245=VECTOR('',#8820,0.41);
#2246=VECTOR('',#8829,0.26);
#2247=VECTOR('',#8834,0.25);
#2248=VECTOR('',#8839,0.225);
#2249=VECTOR('',#8844,1.);
#2250=VECTOR('',#8845,1.);
#2251=VECTOR('',#8846,1.);
#2252=VECTOR('',#8847,1.);
#2253=VECTOR('',#8850,1.);
#2254=VECTOR('',#8851,1.);
#2255=VECTOR('',#8852,1.);
#2256=VECTOR('',#8855,1.);
#2257=VECTOR('',#8856,1.);
#2258=VECTOR('',#8857,1.);
#2259=VECTOR('',#8860,1.);
#2260=VECTOR('',#8861,1.);
#2261=VECTOR('',#8862,1.);
#2262=VECTOR('',#8865,1.);
#2263=VECTOR('',#8866,1.);
#2264=VECTOR('',#8867,1.);
#2265=VECTOR('',#8870,1.);
#2266=VECTOR('',#8871,1.);
#2267=VECTOR('',#8880,1.);
#2268=VECTOR('',#8881,1.);
#2269=VECTOR('',#8882,1.);
#2270=VECTOR('',#8883,1.);
#2271=VECTOR('',#8886,1.);
#2272=VECTOR('',#8887,1.);
#2273=VECTOR('',#8888,1.);
#2274=VECTOR('',#8891,1.);
#2275=VECTOR('',#8892,1.);
#2276=VECTOR('',#8893,1.);
#2277=VECTOR('',#8896,1.);
#2278=VECTOR('',#8897,1.);
#2279=VECTOR('',#8898,1.);
#2280=VECTOR('',#8901,1.);
#2281=VECTOR('',#8902,1.);
#2282=VECTOR('',#8903,1.);
#2283=VECTOR('',#8906,1.);
#2284=VECTOR('',#8907,1.);
#2285=VECTOR('',#8918,0.235);
#2286=VECTOR('',#8923,0.25);
#2287=VECTOR('',#8928,0.2125);
#2288=VECTOR('',#8935,1.);
#2289=VECTOR('',#8936,1.);
#2290=VECTOR('',#8937,1.);
#2291=VECTOR('',#8938,1.);
#2292=VECTOR('',#8939,1.);
#2293=VECTOR('',#8940,1.);
#2294=VECTOR('',#8941,1.);
#2295=VECTOR('',#8942,1.);
#2296=VECTOR('',#8945,1.);
#2297=VECTOR('',#8946,1.);
#2298=VECTOR('',#8947,1.);
#2299=VECTOR('',#8950,1.);
#2300=VECTOR('',#8951,1.);
#2301=VECTOR('',#8954,1.);
#2302=VECTOR('',#8955,1.);
#2303=VECTOR('',#8958,1.);
#2304=VECTOR('',#8959,1.);
#2305=VECTOR('',#8962,1.);
#2306=VECTOR('',#8963,1.);
#2307=VECTOR('',#8964,1.);
#2308=VECTOR('',#8965,1.);
#2309=VECTOR('',#8968,1.);
#2310=VECTOR('',#8971,1.);
#2311=VECTOR('',#8974,1.);
#2312=VECTOR('',#8983,0.42);
#2313=VECTOR('',#8990,0.8);
#2314=VECTOR('',#9001,0.734027674973257);
#2315=VECTOR('',#9008,0.734027674973257);
#2316=VECTOR('',#9011,1.);
#2317=VECTOR('',#9012,1.);
#2318=VECTOR('',#9015,1.);
#2319=VECTOR('',#9018,1.);
#2320=VECTOR('',#9023,0.4);
#2321=VECTOR('',#9028,1.);
#2322=VECTOR('',#9031,1.);
#2323=CIRCLE('',#6463,0.25);
#2324=CIRCLE('',#6464,0.25);
#2325=CIRCLE('',#6466,0.25);
#2326=CIRCLE('',#6467,0.25);
#2327=CIRCLE('',#6476,0.33);
#2328=CIRCLE('',#6477,0.33);
#2329=CIRCLE('',#6479,0.33);
#2330=CIRCLE('',#6480,0.33);
#2331=CIRCLE('',#6482,0.44);
#2332=CIRCLE('',#6483,0.44);
#2333=CIRCLE('',#6485,0.44);
#2334=CIRCLE('',#6486,0.44);
#2335=CIRCLE('',#6488,0.44);
#2336=CIRCLE('',#6489,0.44);
#2337=CIRCLE('',#6491,0.44);
#2338=CIRCLE('',#6492,0.44);
#2339=CIRCLE('',#6494,3.1);
#2340=CIRCLE('',#6495,3.1);
#2341=CIRCLE('',#6506,0.425);
#2342=CIRCLE('',#6507,0.425);
#2343=CIRCLE('',#6509,0.595);
#2344=CIRCLE('',#6510,0.595);
#2345=CIRCLE('',#6515,0.425);
#2346=CIRCLE('',#6516,0.425);
#2347=CIRCLE('',#6518,0.595);
#2348=CIRCLE('',#6519,0.595);
#2349=CIRCLE('',#6524,0.425);
#2350=CIRCLE('',#6525,0.425);
#2351=CIRCLE('',#6527,0.595);
#2352=CIRCLE('',#6528,0.595);
#2353=CIRCLE('',#6533,0.425);
#2354=CIRCLE('',#6534,0.425);
#2355=CIRCLE('',#6536,0.595);
#2356=CIRCLE('',#6537,0.595);
#2357=CIRCLE('',#6564,0.2942);
#2358=CIRCLE('',#6566,0.45);
#2359=CIRCLE('',#6568,0.5);
#2360=CIRCLE('',#6570,0.5);
#2361=CIRCLE('',#6572,0.47);
#2362=CIRCLE('',#6574,0.32);
#2363=CIRCLE('',#6576,0.2942);
#2364=CIRCLE('',#6581,2.05);
#2365=CIRCLE('',#6582,2.05);
#2366=CIRCLE('',#6584,2.05);
#2367=CIRCLE('',#6585,2.05);
#2368=CIRCLE('',#6587,2.35);
#2369=CIRCLE('',#6589,3.);
#2370=CIRCLE('',#6590,3.);
#2371=CIRCLE('',#6592,3.);
#2372=CIRCLE('',#6593,3.);
#2373=CIRCLE('',#6597,0.6);
#2374=CIRCLE('',#6598,0.6);
#2375=CIRCLE('',#6600,0.6);
#2376=CIRCLE('',#6601,0.6);
#2377=CIRCLE('',#6603,0.6);
#2378=CIRCLE('',#6604,0.6);
#2379=CIRCLE('',#6606,0.6);
#2380=CIRCLE('',#6607,0.6);
#2381=CIRCLE('',#6620,1.8);
#2382=CIRCLE('',#6621,1.8);
#2383=CIRCLE('',#6623,2.19089023002066);
#2384=CIRCLE('',#6625,2.35);
#2385=CIRCLE('',#6626,2.19089023002066);
#2386=CIRCLE('',#6631,1.65);
#2387=CIRCLE('',#6632,1.65);
#2388=CIRCLE('',#6638,1.);
#2389=CIRCLE('',#6640,1.75);
#2390=CIRCLE('',#6642,1.75);
#2391=CIRCLE('',#6644,1.);
#2392=CIRCLE('',#6650,0.6);
#2393=CIRCLE('',#6652,0.65);
#2394=CIRCLE('',#6654,0.65);
#2395=CIRCLE('',#6656,0.62);
#2396=CIRCLE('',#6658,0.42);
#2397=CIRCLE('',#6660,0.3933);
#2398=CIRCLE('',#6662,0.3933);
#2399=CIRCLE('',#6664,0.32);
#2400=CIRCLE('',#6678,1.);
#2401=CIRCLE('',#6682,1.);
#2402=CIRCLE('',#6684,0.21);
#2403=CIRCLE('',#6685,0.21);
#2404=CIRCLE('',#6689,0.6);
#2405=CIRCLE('',#6693,0.6);
#2406=CIRCLE('',#6695,0.4);
#2407=CIRCLE('',#6696,0.4);
#2408=CIRCLE('',#6699,0.6);
#2409=CIRCLE('',#6700,0.6);
#2410=CIRCLE('',#6703,1.);
#2411=CIRCLE('',#6704,1.);
#2412=CIRCLE('',#6709,0.605);
#2413=CIRCLE('',#6710,0.605);
#2414=CIRCLE('',#6712,0.9);
#2415=CIRCLE('',#6713,0.9);
#2416=CIRCLE('',#6718,0.605);
#2417=CIRCLE('',#6719,0.605);
#2418=CIRCLE('',#6721,0.9);
#2419=CIRCLE('',#6722,0.9);
#2420=CIRCLE('',#6727,0.275);
#2421=CIRCLE('',#6728,0.275);
#2422=CIRCLE('',#6730,1.);
#2423=CIRCLE('',#6731,1.);
#2424=CIRCLE('',#6736,0.21);
#2425=CIRCLE('',#6738,0.21);
#2426=CIRCLE('',#6739,0.21);
#2427=CIRCLE('',#6742,1.005);
#2428=CIRCLE('',#6743,1.005);
#2429=CIRCLE('',#6745,1.5);
#2430=CIRCLE('',#6746,1.5);
#2431=CIRCLE('',#6751,0.21);
#2432=CIRCLE('',#6753,0.21);
#2433=CIRCLE('',#6754,0.21);
#2434=CIRCLE('',#6757,1.005);
#2435=CIRCLE('',#6758,1.005);
#2436=CIRCLE('',#6760,1.5);
#2437=CIRCLE('',#6761,1.5);
#2438=CIRCLE('',#6769,6.);
#2439=CIRCLE('',#6770,0.33);
#2440=CIRCLE('',#6771,0.33);
#2441=CIRCLE('',#6772,0.33);
#2442=CIRCLE('',#6773,0.33);
#2443=CIRCLE('',#6774,0.33);
#2444=CIRCLE('',#6775,0.33);
#2445=CIRCLE('',#6776,1.);
#2446=CIRCLE('',#6778,1.);
#2447=CIRCLE('',#6780,0.33);
#2448=CIRCLE('',#6782,0.33);
#2449=CIRCLE('',#6784,0.33);
#2450=CIRCLE('',#6786,0.33);
#2451=CIRCLE('',#6788,0.33);
#2452=CIRCLE('',#6790,0.33);
#2453=CIRCLE('',#6792,6.);
#2454=CIRCLE('',#6793,1.8);
#2455=CIRCLE('',#6796,1.8);
#2456=CIRCLE('',#6800,0.425);
#2457=CIRCLE('',#6801,0.425);
#2458=CIRCLE('',#6803,1.4);
#2459=CIRCLE('',#6804,1.4);
#2460=CIRCLE('',#6810,0.125);
#2461=CIRCLE('',#6813,1.4);
#2462=CIRCLE('',#6814,0.6);
#2463=CIRCLE('',#6816,0.6);
#2464=CIRCLE('',#6820,1.);
#2465=CIRCLE('',#6821,1.);
#2466=CIRCLE('',#6826,1.4);
#2467=CIRCLE('',#6827,0.0555000000000001);
#2468=CIRCLE('',#6828,1.24783954473516);
#2469=CIRCLE('',#6829,0.0555000000000001);
#2470=CIRCLE('',#6830,1.24783954473516);
#2471=CIRCLE('',#6831,0.0555000000000001);
#2472=CIRCLE('',#6832,1.24783954473516);
#2473=CIRCLE('',#6833,0.0555000000000001);
#2474=CIRCLE('',#6834,1.24783954473516);
#2475=CIRCLE('',#6835,0.0555000000000001);
#2476=CIRCLE('',#6836,1.24783954473516);
#2477=CIRCLE('',#6837,0.0555000000000001);
#2478=CIRCLE('',#6838,1.24783954473516);
#2479=CIRCLE('',#6839,0.0555000000000001);
#2480=CIRCLE('',#6840,1.24783954473516);
#2481=CIRCLE('',#6841,0.0555000000000001);
#2482=CIRCLE('',#6842,1.24783954473516);
#2483=CIRCLE('',#6843,0.0555000000000001);
#2484=CIRCLE('',#6844,1.24783954473516);
#2485=CIRCLE('',#6845,0.0555000000000001);
#2486=CIRCLE('',#6846,1.24783954473516);
#2487=CIRCLE('',#6847,0.0555000000000001);
#2488=CIRCLE('',#6848,1.24783954473516);
#2489=CIRCLE('',#6849,0.0555000000000001);
#2490=CIRCLE('',#6850,1.24783954473516);
#2491=CIRCLE('',#6851,0.0555000000000001);
#2492=CIRCLE('',#6852,1.24783954473516);
#2493=CIRCLE('',#6853,0.0555000000000001);
#2494=CIRCLE('',#6854,1.24783954473516);
#2495=CIRCLE('',#6855,0.0555000000000001);
#2496=CIRCLE('',#6856,1.24783954473516);
#2497=CIRCLE('',#6857,0.0555000000000001);
#2498=CIRCLE('',#6858,1.24783954473516);
#2499=CIRCLE('',#6859,0.0555000000000001);
#2500=CIRCLE('',#6860,1.24783954473516);
#2501=CIRCLE('',#6861,0.0555000000000001);
#2502=CIRCLE('',#6862,1.24783954473516);
#2503=CIRCLE('',#6863,0.0555000000000001);
#2504=CIRCLE('',#6864,1.24783954473516);
#2505=CIRCLE('',#6865,0.0555000000000001);
#2506=CIRCLE('',#6866,1.24783954473516);
#2507=CIRCLE('',#6867,0.0555000000000001);
#2508=CIRCLE('',#6868,1.24783954473516);
#2509=CIRCLE('',#6869,0.0555000000000001);
#2510=CIRCLE('',#6870,1.24783954473516);
#2511=CIRCLE('',#6871,0.0555000000000001);
#2512=CIRCLE('',#6872,1.24783954473516);
#2513=CIRCLE('',#6873,0.0555000000000001);
#2514=CIRCLE('',#6874,1.24783954473516);
#2515=CIRCLE('',#6875,0.0555000000000001);
#2516=CIRCLE('',#6876,1.24783954473516);
#2517=CIRCLE('',#6877,0.0555000000000001);
#2518=CIRCLE('',#6878,1.24783954473516);
#2519=CIRCLE('',#6879,0.0555000000000001);
#2520=CIRCLE('',#6880,1.24783954473516);
#2521=CIRCLE('',#6881,0.0555000000000001);
#2522=CIRCLE('',#6882,1.24783954473516);
#2523=CIRCLE('',#6883,0.0555000000000001);
#2524=CIRCLE('',#6884,1.24783954473516);
#2525=CIRCLE('',#6885,0.0555000000000001);
#2526=CIRCLE('',#6886,1.24783954473516);
#2527=CIRCLE('',#6887,0.0555000000000001);
#2528=CIRCLE('',#6888,1.24783954473516);
#2529=CIRCLE('',#6889,0.0555000000000001);
#2530=CIRCLE('',#6890,1.24783954473516);
#2531=CIRCLE('',#6891,0.0555000000000001);
#2532=CIRCLE('',#6892,1.24783954473516);
#2533=CIRCLE('',#6893,0.0555000000000001);
#2534=CIRCLE('',#6894,1.24783954473516);
#2535=CIRCLE('',#6895,0.0555000000000001);
#2536=CIRCLE('',#6896,1.24783954473516);
#2537=CIRCLE('',#6897,0.0555000000000001);
#2538=CIRCLE('',#6898,1.24783954473516);
#2539=CIRCLE('',#6899,0.0555000000000001);
#2540=CIRCLE('',#6900,1.24783954473516);
#2541=CIRCLE('',#6901,0.0555000000000001);
#2542=CIRCLE('',#6902,1.24783954473516);
#2543=CIRCLE('',#6903,0.0555000000000001);
#2544=CIRCLE('',#6904,1.24783954473516);
#2545=CIRCLE('',#6905,0.0555000000000001);
#2546=CIRCLE('',#6906,1.24783954473516);
#2547=CIRCLE('',#6908,1.4);
#2548=CIRCLE('',#6911,1.4);
#2549=CIRCLE('',#6912,0.0555000000000001);
#2550=CIRCLE('',#6913,1.24783954473516);
#2551=CIRCLE('',#6914,0.0555000000000001);
#2552=CIRCLE('',#6915,1.24783954473516);
#2553=CIRCLE('',#6916,0.0555000000000001);
#2554=CIRCLE('',#6917,1.24783954473516);
#2555=CIRCLE('',#6918,0.0555000000000001);
#2556=CIRCLE('',#6919,1.24783954473516);
#2557=CIRCLE('',#6920,0.0555000000000001);
#2558=CIRCLE('',#6921,1.24783954473516);
#2559=CIRCLE('',#6922,0.0555000000000001);
#2560=CIRCLE('',#6923,1.24783954473516);
#2561=CIRCLE('',#6924,0.0555000000000001);
#2562=CIRCLE('',#6925,1.24783954473516);
#2563=CIRCLE('',#6926,0.0555000000000001);
#2564=CIRCLE('',#6927,1.24783954473516);
#2565=CIRCLE('',#6928,0.0555000000000001);
#2566=CIRCLE('',#6929,1.24783954473516);
#2567=CIRCLE('',#6930,0.0555000000000001);
#2568=CIRCLE('',#6931,1.24783954473516);
#2569=CIRCLE('',#6932,0.0555000000000001);
#2570=CIRCLE('',#6933,1.24783954473516);
#2571=CIRCLE('',#6934,0.0555000000000001);
#2572=CIRCLE('',#6935,1.24783954473516);
#2573=CIRCLE('',#6936,0.0555000000000001);
#2574=CIRCLE('',#6937,1.24783954473516);
#2575=CIRCLE('',#6938,0.0555000000000001);
#2576=CIRCLE('',#6939,1.24783954473516);
#2577=CIRCLE('',#6940,0.0555000000000001);
#2578=CIRCLE('',#6941,1.24783954473516);
#2579=CIRCLE('',#6942,0.0555000000000001);
#2580=CIRCLE('',#6943,1.24783954473516);
#2581=CIRCLE('',#6944,0.0555000000000001);
#2582=CIRCLE('',#6945,1.24783954473516);
#2583=CIRCLE('',#6946,0.0555000000000001);
#2584=CIRCLE('',#6947,1.24783954473516);
#2585=CIRCLE('',#6948,0.0555000000000001);
#2586=CIRCLE('',#6949,1.24783954473516);
#2587=CIRCLE('',#6950,0.0555000000000001);
#2588=CIRCLE('',#6951,1.24783954473516);
#2589=CIRCLE('',#6952,0.0555000000000001);
#2590=CIRCLE('',#6953,1.24783954473516);
#2591=CIRCLE('',#6954,0.0555000000000001);
#2592=CIRCLE('',#6955,1.24783954473516);
#2593=CIRCLE('',#6956,0.0555000000000001);
#2594=CIRCLE('',#6957,1.24783954473516);
#2595=CIRCLE('',#6958,0.0555000000000001);
#2596=CIRCLE('',#6959,1.24783954473516);
#2597=CIRCLE('',#6960,0.0555000000000001);
#2598=CIRCLE('',#6961,1.24783954473516);
#2599=CIRCLE('',#6962,0.0555000000000001);
#2600=CIRCLE('',#6963,1.24783954473516);
#2601=CIRCLE('',#6964,0.0555000000000001);
#2602=CIRCLE('',#6965,1.24783954473516);
#2603=CIRCLE('',#6966,0.0555000000000001);
#2604=CIRCLE('',#6967,1.24783954473516);
#2605=CIRCLE('',#6968,0.0555000000000001);
#2606=CIRCLE('',#6969,1.24783954473516);
#2607=CIRCLE('',#6970,0.0555000000000001);
#2608=CIRCLE('',#6971,1.24783954473516);
#2609=CIRCLE('',#6972,0.0555000000000001);
#2610=CIRCLE('',#6973,1.24783954473516);
#2611=CIRCLE('',#6974,0.0555000000000001);
#2612=CIRCLE('',#6975,1.24783954473516);
#2613=CIRCLE('',#6976,0.0555000000000001);
#2614=CIRCLE('',#6977,1.24783954473516);
#2615=CIRCLE('',#6978,0.0555000000000001);
#2616=CIRCLE('',#6979,1.24783954473516);
#2617=CIRCLE('',#6980,0.0555000000000001);
#2618=CIRCLE('',#6981,1.24783954473516);
#2619=CIRCLE('',#6982,0.0555000000000001);
#2620=CIRCLE('',#6983,1.24783954473516);
#2621=CIRCLE('',#6984,0.0555000000000001);
#2622=CIRCLE('',#6985,1.24783954473516);
#2623=CIRCLE('',#6986,0.0555000000000001);
#2624=CIRCLE('',#6987,1.24783954473516);
#2625=CIRCLE('',#6988,0.0555000000000001);
#2626=CIRCLE('',#6989,1.24783954473516);
#2627=CIRCLE('',#6990,0.0555000000000001);
#2628=CIRCLE('',#6991,1.24783954473516);
#2629=CIRCLE('',#7086,0.375);
#2630=CIRCLE('',#7088,0.425);
#2631=CIRCLE('',#7090,0.425);
#2632=CIRCLE('',#7092,0.395);
#2633=CIRCLE('',#7094,0.27);
#2634=CIRCLE('',#7096,0.24505);
#2635=CIRCLE('',#7098,0.24505);
#2636=CIRCLE('',#7100,0.2);
#2637=CIRCLE('',#7119,0.22);
#2638=CIRCLE('',#7121,0.24505);
#2639=CIRCLE('',#7123,0.24505);
#2640=CIRCLE('',#7125,0.175);
#2641=CIRCLE('',#7140,0.42);
#2642=CIRCLE('',#7141,0.42);
#2643=CIRCLE('',#7143,0.8);
#2644=CIRCLE('',#7144,0.8);
#2645=CIRCLE('',#7149,0.6175);
#2646=CIRCLE('',#7151,0.6175);
#2647=CIRCLE('',#7156,0.338975);
#2648=CIRCLE('',#7157,0.338975);
#2649=VERTEX_POINT('',#9132);
#2650=VERTEX_POINT('',#9134);
#2651=VERTEX_POINT('',#9138);
#2652=VERTEX_POINT('',#9140);
#2653=VERTEX_POINT('',#9144);
#2654=VERTEX_POINT('',#9145);
#2655=VERTEX_POINT('',#9147);
#2656=VERTEX_POINT('',#9149);
#2657=VERTEX_POINT('',#9153);
#2658=VERTEX_POINT('',#9155);
#2659=VERTEX_POINT('',#9159);
#2660=VERTEX_POINT('',#9161);
#2661=VERTEX_POINT('',#9171);
#2662=VERTEX_POINT('',#9173);
#2663=VERTEX_POINT('',#9177);
#2664=VERTEX_POINT('',#9179);
#2665=VERTEX_POINT('',#9183);
#2666=VERTEX_POINT('',#9185);
#2667=VERTEX_POINT('',#9189);
#2668=VERTEX_POINT('',#9191);
#2669=VERTEX_POINT('',#9195);
#2670=VERTEX_POINT('',#9197);
#2671=VERTEX_POINT('',#9201);
#2672=VERTEX_POINT('',#9203);
#2673=VERTEX_POINT('',#9207);
#2674=VERTEX_POINT('',#9209);
#2675=VERTEX_POINT('',#9213);
#2676=VERTEX_POINT('',#9214);
#2677=VERTEX_POINT('',#9216);
#2678=VERTEX_POINT('',#9218);
#2679=VERTEX_POINT('',#9222);
#2680=VERTEX_POINT('',#9224);
#2681=VERTEX_POINT('',#9228);
#2682=VERTEX_POINT('',#9229);
#2683=VERTEX_POINT('',#9231);
#2684=VERTEX_POINT('',#9233);
#2685=VERTEX_POINT('',#9237);
#2686=VERTEX_POINT('',#9242);
#2687=VERTEX_POINT('',#9252);
#2688=VERTEX_POINT('',#9254);
#2689=VERTEX_POINT('',#9258);
#2690=VERTEX_POINT('',#9260);
#2691=VERTEX_POINT('',#9267);
#2692=VERTEX_POINT('',#9269);
#2693=VERTEX_POINT('',#9273);
#2694=VERTEX_POINT('',#9275);
#2695=VERTEX_POINT('',#9282);
#2696=VERTEX_POINT('',#9284);
#2697=VERTEX_POINT('',#9288);
#2698=VERTEX_POINT('',#9290);
#2699=VERTEX_POINT('',#9297);
#2700=VERTEX_POINT('',#9299);
#2701=VERTEX_POINT('',#9303);
#2702=VERTEX_POINT('',#9305);
#2703=VERTEX_POINT('',#9312);
#2704=VERTEX_POINT('',#9313);
#2705=VERTEX_POINT('',#9315);
#2706=VERTEX_POINT('',#9317);
#2707=VERTEX_POINT('',#9321);
#2708=VERTEX_POINT('',#9323);
#2709=VERTEX_POINT('',#9327);
#2710=VERTEX_POINT('',#9329);
#2711=VERTEX_POINT('',#9339);
#2712=VERTEX_POINT('',#9340);
#2713=VERTEX_POINT('',#9342);
#2714=VERTEX_POINT('',#9344);
#2715=VERTEX_POINT('',#9348);
#2716=VERTEX_POINT('',#9350);
#2717=VERTEX_POINT('',#9354);
#2718=VERTEX_POINT('',#9356);
#2719=VERTEX_POINT('',#9366);
#2720=VERTEX_POINT('',#9367);
#2721=VERTEX_POINT('',#9369);
#2722=VERTEX_POINT('',#9371);
#2723=VERTEX_POINT('',#9375);
#2724=VERTEX_POINT('',#9377);
#2725=VERTEX_POINT('',#9381);
#2726=VERTEX_POINT('',#9383);
#2727=VERTEX_POINT('',#9387);
#2728=VERTEX_POINT('',#9389);
#2729=VERTEX_POINT('',#9393);
#2730=VERTEX_POINT('',#9395);
#2731=VERTEX_POINT('',#9404);
#2732=VERTEX_POINT('',#9407);
#2733=VERTEX_POINT('',#9410);
#2734=VERTEX_POINT('',#9414);
#2735=VERTEX_POINT('',#9418);
#2736=VERTEX_POINT('',#9422);
#2737=VERTEX_POINT('',#9425);
#2738=VERTEX_POINT('',#9433);
#2739=VERTEX_POINT('',#9435);
#2740=VERTEX_POINT('',#9439);
#2741=VERTEX_POINT('',#9441);
#2742=VERTEX_POINT('',#9445);
#2743=VERTEX_POINT('',#9446);
#2744=VERTEX_POINT('',#9449);
#2745=VERTEX_POINT('',#9451);
#2746=VERTEX_POINT('',#9455);
#2747=VERTEX_POINT('',#9457);
#2748=VERTEX_POINT('',#9463);
#2749=VERTEX_POINT('',#9465);
#2750=VERTEX_POINT('',#9469);
#2751=VERTEX_POINT('',#9471);
#2752=VERTEX_POINT('',#9475);
#2753=VERTEX_POINT('',#9477);
#2754=VERTEX_POINT('',#9481);
#2755=VERTEX_POINT('',#9483);
#2756=VERTEX_POINT('',#9487);
#2757=VERTEX_POINT('',#9488);
#2758=VERTEX_POINT('',#9490);
#2759=VERTEX_POINT('',#9492);
#2760=VERTEX_POINT('',#9496);
#2761=VERTEX_POINT('',#9498);
#2762=VERTEX_POINT('',#9502);
#2763=VERTEX_POINT('',#9504);
#2764=VERTEX_POINT('',#9508);
#2765=VERTEX_POINT('',#9510);
#2766=VERTEX_POINT('',#9514);
#2767=VERTEX_POINT('',#9516);
#2768=VERTEX_POINT('',#9520);
#2769=VERTEX_POINT('',#9522);
#2770=VERTEX_POINT('',#9526);
#2771=VERTEX_POINT('',#9528);
#2772=VERTEX_POINT('',#9538);
#2773=VERTEX_POINT('',#9540);
#2774=VERTEX_POINT('',#9544);
#2775=VERTEX_POINT('',#9547);
#2776=VERTEX_POINT('',#9548);
#2777=VERTEX_POINT('',#9550);
#2778=VERTEX_POINT('',#9554);
#2779=VERTEX_POINT('',#9555);
#2780=VERTEX_POINT('',#9566);
#2781=VERTEX_POINT('',#9595);
#2782=VERTEX_POINT('',#9632);
#2783=VERTEX_POINT('',#9667);
#2784=VERTEX_POINT('',#9669);
#2785=VERTEX_POINT('',#9680);
#2786=VERTEX_POINT('',#9710);
#2787=VERTEX_POINT('',#9712);
#2788=VERTEX_POINT('',#9715);
#2789=VERTEX_POINT('',#9716);
#2790=VERTEX_POINT('',#9735);
#2791=VERTEX_POINT('',#9756);
#2792=VERTEX_POINT('',#9757);
#2793=VERTEX_POINT('',#9776);
#2794=VERTEX_POINT('',#9797);
#2795=VERTEX_POINT('',#9798);
#2796=VERTEX_POINT('',#9817);
#2797=VERTEX_POINT('',#9838);
#2798=VERTEX_POINT('',#9839);
#2799=VERTEX_POINT('',#9858);
#2800=VERTEX_POINT('',#9880);
#2801=VERTEX_POINT('',#9917);
#2802=VERTEX_POINT('',#9954);
#2803=VERTEX_POINT('',#9991);
#2804=VERTEX_POINT('',#10028);
#2805=VERTEX_POINT('',#10031);
#2806=VERTEX_POINT('',#10034);
#2807=VERTEX_POINT('',#10038);
#2808=VERTEX_POINT('',#10046);
#2809=VERTEX_POINT('',#10049);
#2810=VERTEX_POINT('',#10053);
#2811=VERTEX_POINT('',#10057);
#2812=VERTEX_POINT('',#10061);
#2813=VERTEX_POINT('',#10064);
#2814=VERTEX_POINT('',#10068);
#2815=VERTEX_POINT('',#10072);
#2816=VERTEX_POINT('',#10077);
#2817=VERTEX_POINT('',#10078);
#2818=VERTEX_POINT('',#10080);
#2819=VERTEX_POINT('',#10082);
#2820=VERTEX_POINT('',#10086);
#2821=VERTEX_POINT('',#10088);
#2822=VERTEX_POINT('',#10092);
#2823=VERTEX_POINT('',#10094);
#2824=VERTEX_POINT('',#10098);
#2825=VERTEX_POINT('',#10100);
#2826=VERTEX_POINT('',#10104);
#2827=VERTEX_POINT('',#10106);
#2828=VERTEX_POINT('',#10117);
#2829=VERTEX_POINT('',#10118);
#2830=VERTEX_POINT('',#10120);
#2831=VERTEX_POINT('',#10122);
#2832=VERTEX_POINT('',#10126);
#2833=VERTEX_POINT('',#10128);
#2834=VERTEX_POINT('',#10132);
#2835=VERTEX_POINT('',#10134);
#2836=VERTEX_POINT('',#10142);
#2837=VERTEX_POINT('',#10144);
#2838=VERTEX_POINT('',#10149);
#2839=VERTEX_POINT('',#10150);
#2840=VERTEX_POINT('',#10152);
#2841=VERTEX_POINT('',#10154);
#2842=VERTEX_POINT('',#10158);
#2843=VERTEX_POINT('',#10160);
#2844=VERTEX_POINT('',#10164);
#2845=VERTEX_POINT('',#10166);
#2846=VERTEX_POINT('',#10174);
#2847=VERTEX_POINT('',#10176);
#2848=VERTEX_POINT('',#10181);
#2849=VERTEX_POINT('',#10183);
#2850=VERTEX_POINT('',#10188);
#2851=VERTEX_POINT('',#10190);
#2852=VERTEX_POINT('',#10197);
#2853=VERTEX_POINT('',#10199);
#2854=VERTEX_POINT('',#10203);
#2855=VERTEX_POINT('',#10205);
#2856=VERTEX_POINT('',#10212);
#2857=VERTEX_POINT('',#10214);
#2858=VERTEX_POINT('',#10218);
#2859=VERTEX_POINT('',#10220);
#2860=VERTEX_POINT('',#10227);
#2861=VERTEX_POINT('',#10229);
#2862=VERTEX_POINT('',#10233);
#2863=VERTEX_POINT('',#10235);
#2864=VERTEX_POINT('',#10242);
#2865=VERTEX_POINT('',#10243);
#2866=VERTEX_POINT('',#10247);
#2867=VERTEX_POINT('',#10262);
#2868=VERTEX_POINT('',#10264);
#2869=VERTEX_POINT('',#10266);
#2870=VERTEX_POINT('',#10303);
#2871=VERTEX_POINT('',#10322);
#2872=VERTEX_POINT('',#10324);
#2873=VERTEX_POINT('',#10328);
#2874=VERTEX_POINT('',#10330);
#2875=VERTEX_POINT('',#10337);
#2876=VERTEX_POINT('',#10338);
#2877=VERTEX_POINT('',#10342);
#2878=VERTEX_POINT('',#10357);
#2879=VERTEX_POINT('',#10359);
#2880=VERTEX_POINT('',#10361);
#2881=VERTEX_POINT('',#10398);
#2882=VERTEX_POINT('',#10417);
#2883=VERTEX_POINT('',#10419);
#2884=VERTEX_POINT('',#10423);
#2885=VERTEX_POINT('',#10425);
#2886=VERTEX_POINT('',#10432);
#2887=VERTEX_POINT('',#10433);
#2888=VERTEX_POINT('',#10435);
#2889=VERTEX_POINT('',#10437);
#2890=VERTEX_POINT('',#10441);
#2891=VERTEX_POINT('',#10443);
#2892=VERTEX_POINT('',#10447);
#2893=VERTEX_POINT('',#10449);
#2894=VERTEX_POINT('',#10453);
#2895=VERTEX_POINT('',#10455);
#2896=VERTEX_POINT('',#10457);
#2897=VERTEX_POINT('',#10459);
#2898=VERTEX_POINT('',#10461);
#2899=VERTEX_POINT('',#10463);
#2900=VERTEX_POINT('',#10465);
#2901=VERTEX_POINT('',#10471);
#2902=VERTEX_POINT('',#10475);
#2903=VERTEX_POINT('',#10479);
#2904=VERTEX_POINT('',#10483);
#2905=VERTEX_POINT('',#10487);
#2906=VERTEX_POINT('',#10491);
#2907=VERTEX_POINT('',#10495);
#2908=VERTEX_POINT('',#10497);
#2909=VERTEX_POINT('',#10502);
#2910=VERTEX_POINT('',#10508);
#2911=VERTEX_POINT('',#10510);
#2912=VERTEX_POINT('',#10514);
#2913=VERTEX_POINT('',#10516);
#2914=VERTEX_POINT('',#10523);
#2915=VERTEX_POINT('',#10524);
#2916=VERTEX_POINT('',#10526);
#2917=VERTEX_POINT('',#10528);
#2918=VERTEX_POINT('',#10532);
#2919=VERTEX_POINT('',#10534);
#2920=VERTEX_POINT('',#10537);
#2921=VERTEX_POINT('',#10540);
#2922=VERTEX_POINT('',#10542);
#2923=VERTEX_POINT('',#10546);
#2924=VERTEX_POINT('',#10551);
#2925=VERTEX_POINT('',#10552);
#2926=VERTEX_POINT('',#10589);
#2927=VERTEX_POINT('',#10590);
#2928=VERTEX_POINT('',#10627);
#2929=VERTEX_POINT('',#10628);
#2930=VERTEX_POINT('',#10666);
#2931=VERTEX_POINT('',#10667);
#2932=VERTEX_POINT('',#10678);
#2933=VERTEX_POINT('',#10709);
#2934=VERTEX_POINT('',#10711);
#2935=VERTEX_POINT('',#10722);
#2936=VERTEX_POINT('',#10752);
#2937=VERTEX_POINT('',#10755);
#2938=VERTEX_POINT('',#10758);
#2939=VERTEX_POINT('',#10759);
#2940=VERTEX_POINT('',#10778);
#2941=VERTEX_POINT('',#10799);
#2942=VERTEX_POINT('',#10800);
#2943=VERTEX_POINT('',#10819);
#2944=VERTEX_POINT('',#10846);
#2945=VERTEX_POINT('',#10848);
#2946=VERTEX_POINT('',#10849);
#2947=VERTEX_POINT('',#10851);
#2948=VERTEX_POINT('',#10853);
#2949=VERTEX_POINT('',#10855);
#2950=VERTEX_POINT('',#10857);
#2951=VERTEX_POINT('',#10859);
#2952=VERTEX_POINT('',#10861);
#2953=VERTEX_POINT('',#10863);
#2954=VERTEX_POINT('',#10865);
#2955=VERTEX_POINT('',#10867);
#2956=VERTEX_POINT('',#10869);
#2957=VERTEX_POINT('',#10871);
#2958=VERTEX_POINT('',#10873);
#2959=VERTEX_POINT('',#10875);
#2960=VERTEX_POINT('',#10877);
#2961=VERTEX_POINT('',#10879);
#2962=VERTEX_POINT('',#10881);
#2963=VERTEX_POINT('',#10883);
#2964=VERTEX_POINT('',#10885);
#2965=VERTEX_POINT('',#10887);
#2966=VERTEX_POINT('',#10889);
#2967=VERTEX_POINT('',#10891);
#2968=VERTEX_POINT('',#10893);
#2969=VERTEX_POINT('',#10895);
#2970=VERTEX_POINT('',#10897);
#2971=VERTEX_POINT('',#10899);
#2972=VERTEX_POINT('',#10901);
#2973=VERTEX_POINT('',#10903);
#2974=VERTEX_POINT('',#10905);
#2975=VERTEX_POINT('',#10907);
#2976=VERTEX_POINT('',#10909);
#2977=VERTEX_POINT('',#10911);
#2978=VERTEX_POINT('',#10913);
#2979=VERTEX_POINT('',#10915);
#2980=VERTEX_POINT('',#10917);
#2981=VERTEX_POINT('',#10919);
#2982=VERTEX_POINT('',#10921);
#2983=VERTEX_POINT('',#10923);
#2984=VERTEX_POINT('',#10925);
#2985=VERTEX_POINT('',#10927);
#2986=VERTEX_POINT('',#10929);
#2987=VERTEX_POINT('',#10931);
#2988=VERTEX_POINT('',#10933);
#2989=VERTEX_POINT('',#10935);
#2990=VERTEX_POINT('',#10937);
#2991=VERTEX_POINT('',#10939);
#2992=VERTEX_POINT('',#10941);
#2993=VERTEX_POINT('',#10943);
#2994=VERTEX_POINT('',#10945);
#2995=VERTEX_POINT('',#10947);
#2996=VERTEX_POINT('',#10949);
#2997=VERTEX_POINT('',#10951);
#2998=VERTEX_POINT('',#10953);
#2999=VERTEX_POINT('',#10955);
#3000=VERTEX_POINT('',#10957);
#3001=VERTEX_POINT('',#10959);
#3002=VERTEX_POINT('',#10961);
#3003=VERTEX_POINT('',#10963);
#3004=VERTEX_POINT('',#10965);
#3005=VERTEX_POINT('',#10967);
#3006=VERTEX_POINT('',#10969);
#3007=VERTEX_POINT('',#10971);
#3008=VERTEX_POINT('',#10973);
#3009=VERTEX_POINT('',#10975);
#3010=VERTEX_POINT('',#10977);
#3011=VERTEX_POINT('',#10979);
#3012=VERTEX_POINT('',#10981);
#3013=VERTEX_POINT('',#10983);
#3014=VERTEX_POINT('',#10985);
#3015=VERTEX_POINT('',#10987);
#3016=VERTEX_POINT('',#10989);
#3017=VERTEX_POINT('',#10991);
#3018=VERTEX_POINT('',#10993);
#3019=VERTEX_POINT('',#10995);
#3020=VERTEX_POINT('',#10997);
#3021=VERTEX_POINT('',#10999);
#3022=VERTEX_POINT('',#11001);
#3023=VERTEX_POINT('',#11003);
#3024=VERTEX_POINT('',#11005);
#3025=VERTEX_POINT('',#11009);
#3026=VERTEX_POINT('',#11014);
#3027=VERTEX_POINT('',#11016);
#3028=VERTEX_POINT('',#11017);
#3029=VERTEX_POINT('',#11019);
#3030=VERTEX_POINT('',#11021);
#3031=VERTEX_POINT('',#11023);
#3032=VERTEX_POINT('',#11025);
#3033=VERTEX_POINT('',#11027);
#3034=VERTEX_POINT('',#11029);
#3035=VERTEX_POINT('',#11031);
#3036=VERTEX_POINT('',#11033);
#3037=VERTEX_POINT('',#11035);
#3038=VERTEX_POINT('',#11037);
#3039=VERTEX_POINT('',#11039);
#3040=VERTEX_POINT('',#11041);
#3041=VERTEX_POINT('',#11043);
#3042=VERTEX_POINT('',#11045);
#3043=VERTEX_POINT('',#11047);
#3044=VERTEX_POINT('',#11049);
#3045=VERTEX_POINT('',#11051);
#3046=VERTEX_POINT('',#11053);
#3047=VERTEX_POINT('',#11055);
#3048=VERTEX_POINT('',#11057);
#3049=VERTEX_POINT('',#11059);
#3050=VERTEX_POINT('',#11061);
#3051=VERTEX_POINT('',#11063);
#3052=VERTEX_POINT('',#11065);
#3053=VERTEX_POINT('',#11067);
#3054=VERTEX_POINT('',#11069);
#3055=VERTEX_POINT('',#11071);
#3056=VERTEX_POINT('',#11073);
#3057=VERTEX_POINT('',#11075);
#3058=VERTEX_POINT('',#11077);
#3059=VERTEX_POINT('',#11079);
#3060=VERTEX_POINT('',#11081);
#3061=VERTEX_POINT('',#11083);
#3062=VERTEX_POINT('',#11085);
#3063=VERTEX_POINT('',#11087);
#3064=VERTEX_POINT('',#11089);
#3065=VERTEX_POINT('',#11091);
#3066=VERTEX_POINT('',#11093);
#3067=VERTEX_POINT('',#11095);
#3068=VERTEX_POINT('',#11097);
#3069=VERTEX_POINT('',#11099);
#3070=VERTEX_POINT('',#11101);
#3071=VERTEX_POINT('',#11103);
#3072=VERTEX_POINT('',#11105);
#3073=VERTEX_POINT('',#11107);
#3074=VERTEX_POINT('',#11109);
#3075=VERTEX_POINT('',#11111);
#3076=VERTEX_POINT('',#11113);
#3077=VERTEX_POINT('',#11115);
#3078=VERTEX_POINT('',#11117);
#3079=VERTEX_POINT('',#11119);
#3080=VERTEX_POINT('',#11121);
#3081=VERTEX_POINT('',#11123);
#3082=VERTEX_POINT('',#11125);
#3083=VERTEX_POINT('',#11127);
#3084=VERTEX_POINT('',#11129);
#3085=VERTEX_POINT('',#11131);
#3086=VERTEX_POINT('',#11133);
#3087=VERTEX_POINT('',#11135);
#3088=VERTEX_POINT('',#11137);
#3089=VERTEX_POINT('',#11139);
#3090=VERTEX_POINT('',#11141);
#3091=VERTEX_POINT('',#11143);
#3092=VERTEX_POINT('',#11145);
#3093=VERTEX_POINT('',#11147);
#3094=VERTEX_POINT('',#11149);
#3095=VERTEX_POINT('',#11151);
#3096=VERTEX_POINT('',#11153);
#3097=VERTEX_POINT('',#11155);
#3098=VERTEX_POINT('',#11157);
#3099=VERTEX_POINT('',#11159);
#3100=VERTEX_POINT('',#11161);
#3101=VERTEX_POINT('',#11163);
#3102=VERTEX_POINT('',#11165);
#3103=VERTEX_POINT('',#11167);
#3104=VERTEX_POINT('',#11169);
#3105=VERTEX_POINT('',#11171);
#3106=VERTEX_POINT('',#11173);
#3107=VERTEX_POINT('',#11340);
#3108=VERTEX_POINT('',#11341);
#3109=VERTEX_POINT('',#11343);
#3110=VERTEX_POINT('',#11345);
#3111=VERTEX_POINT('',#11347);
#3112=VERTEX_POINT('',#11349);
#3113=VERTEX_POINT('',#11351);
#3114=VERTEX_POINT('',#11353);
#3115=VERTEX_POINT('',#11357);
#3116=VERTEX_POINT('',#11359);
#3117=VERTEX_POINT('',#11363);
#3118=VERTEX_POINT('',#11367);
#3119=VERTEX_POINT('',#11371);
#3120=VERTEX_POINT('',#11375);
#3121=VERTEX_POINT('',#11377);
#3122=VERTEX_POINT('',#11379);
#3123=VERTEX_POINT('',#11391);
#3124=VERTEX_POINT('',#11394);
#3125=VERTEX_POINT('',#11398);
#3126=VERTEX_POINT('',#11402);
#3127=VERTEX_POINT('',#11406);
#3128=VERTEX_POINT('',#11409);
#3129=VERTEX_POINT('',#11413);
#3130=VERTEX_POINT('',#11417);
#3131=VERTEX_POINT('',#11422);
#3132=VERTEX_POINT('',#11423);
#3133=VERTEX_POINT('',#11425);
#3134=VERTEX_POINT('',#11427);
#3135=VERTEX_POINT('',#11431);
#3136=VERTEX_POINT('',#11433);
#3137=VERTEX_POINT('',#11437);
#3138=VERTEX_POINT('',#11439);
#3139=VERTEX_POINT('',#11443);
#3140=VERTEX_POINT('',#11445);
#3141=VERTEX_POINT('',#11449);
#3142=VERTEX_POINT('',#11451);
#3143=VERTEX_POINT('',#11461);
#3144=VERTEX_POINT('',#11462);
#3145=VERTEX_POINT('',#11464);
#3146=VERTEX_POINT('',#11466);
#3147=VERTEX_POINT('',#11470);
#3148=VERTEX_POINT('',#11472);
#3149=VERTEX_POINT('',#11476);
#3150=VERTEX_POINT('',#11478);
#3151=VERTEX_POINT('',#11482);
#3152=VERTEX_POINT('',#11484);
#3153=VERTEX_POINT('',#11488);
#3154=VERTEX_POINT('',#11490);
#3155=VERTEX_POINT('',#11498);
#3156=VERTEX_POINT('',#11501);
#3157=VERTEX_POINT('',#11505);
#3158=VERTEX_POINT('',#11509);
#3159=VERTEX_POINT('',#11515);
#3160=VERTEX_POINT('',#11516);
#3161=VERTEX_POINT('',#11518);
#3162=VERTEX_POINT('',#11520);
#3163=VERTEX_POINT('',#11522);
#3164=VERTEX_POINT('',#11524);
#3165=VERTEX_POINT('',#11526);
#3166=VERTEX_POINT('',#11528);
#3167=VERTEX_POINT('',#11532);
#3168=VERTEX_POINT('',#11534);
#3169=VERTEX_POINT('',#11538);
#3170=VERTEX_POINT('',#11542);
#3171=VERTEX_POINT('',#11546);
#3172=VERTEX_POINT('',#11550);
#3173=VERTEX_POINT('',#11551);
#3174=VERTEX_POINT('',#11554);
#3175=VERTEX_POINT('',#11566);
#3176=VERTEX_POINT('',#11568);
#3177=VERTEX_POINT('',#11572);
#3178=VERTEX_POINT('',#11574);
#3179=VERTEX_POINT('',#11581);
#3180=VERTEX_POINT('',#11582);
#3181=VERTEX_POINT('',#11586);
#3182=VERTEX_POINT('',#11590);
#3183=VERTEX_POINT('',#11593);
#3184=VERTEX_POINT('',#11597);
#3185=VERTEX_POINT('',#11601);
#3186=VERTEX_POINT('',#11609);
#3187=VERTEX_POINT('',#11611);
#3188=VERTEX_POINT('',#11613);
#3189=VERTEX_POINT('',#11617);
#3190=VERTEX_POINT('',#11621);
#3191=VERTEX_POINT('',#11625);
#3192=VERTEX_POINT('',#11629);
#3193=VERTEX_POINT('',#11644);
#3194=VERTEX_POINT('',#11646);
#3195=EDGE_CURVE('',#2649,#2649,#2323,.T.);
#3196=EDGE_CURVE('',#2649,#2650,#1479,.T.);
#3197=EDGE_CURVE('',#2650,#2650,#2324,.T.);
#3198=EDGE_CURVE('',#2651,#2651,#2325,.T.);
#3199=EDGE_CURVE('',#2651,#2652,#1480,.T.);
#3200=EDGE_CURVE('',#2652,#2652,#2326,.T.);
#3201=EDGE_CURVE('',#2653,#2654,#1481,.T.);
#3202=EDGE_CURVE('',#2654,#2655,#1482,.T.);
#3203=EDGE_CURVE('',#2656,#2655,#1483,.T.);
#3204=EDGE_CURVE('',#2653,#2656,#1484,.T.);
#3205=EDGE_CURVE('',#2657,#2653,#1485,.T.);
#3206=EDGE_CURVE('',#2658,#2656,#1486,.T.);
#3207=EDGE_CURVE('',#2657,#2658,#1487,.T.);
#3208=EDGE_CURVE('',#2659,#2657,#1488,.T.);
#3209=EDGE_CURVE('',#2660,#2658,#1489,.T.);
#3210=EDGE_CURVE('',#2659,#2660,#1490,.T.);
#3211=EDGE_CURVE('',#2654,#2659,#1491,.T.);
#3212=EDGE_CURVE('',#2655,#2660,#1492,.T.);
#3213=EDGE_CURVE('',#2661,#2661,#2327,.T.);
#3214=EDGE_CURVE('',#2661,#2662,#1493,.T.);
#3215=EDGE_CURVE('',#2662,#2662,#2328,.T.);
#3216=EDGE_CURVE('',#2663,#2663,#2329,.T.);
#3217=EDGE_CURVE('',#2663,#2664,#1494,.T.);
#3218=EDGE_CURVE('',#2664,#2664,#2330,.T.);
#3219=EDGE_CURVE('',#2665,#2665,#2331,.T.);
#3220=EDGE_CURVE('',#2665,#2666,#1495,.T.);
#3221=EDGE_CURVE('',#2666,#2666,#2332,.T.);
#3222=EDGE_CURVE('',#2667,#2667,#2333,.T.);
#3223=EDGE_CURVE('',#2667,#2668,#1496,.T.);
#3224=EDGE_CURVE('',#2668,#2668,#2334,.T.);
#3225=EDGE_CURVE('',#2669,#2669,#2335,.T.);
#3226=EDGE_CURVE('',#2669,#2670,#1497,.T.);
#3227=EDGE_CURVE('',#2670,#2670,#2336,.T.);
#3228=EDGE_CURVE('',#2671,#2671,#2337,.T.);
#3229=EDGE_CURVE('',#2671,#2672,#1498,.T.);
#3230=EDGE_CURVE('',#2672,#2672,#2338,.T.);
#3231=EDGE_CURVE('',#2673,#2673,#2339,.T.);
#3232=EDGE_CURVE('',#2673,#2674,#1499,.T.);
#3233=EDGE_CURVE('',#2674,#2674,#2340,.T.);
#3234=EDGE_CURVE('',#2675,#2676,#1500,.T.);
#3235=EDGE_CURVE('',#2677,#2675,#1501,.T.);
#3236=EDGE_CURVE('',#2678,#2677,#1502,.T.);
#3237=EDGE_CURVE('',#2678,#2676,#1503,.T.);
#3238=EDGE_CURVE('',#2677,#2679,#1504,.T.);
#3239=EDGE_CURVE('',#2679,#2680,#1505,.T.);
#3240=EDGE_CURVE('',#2680,#2678,#1506,.T.);
#3241=EDGE_CURVE('',#2681,#2682,#1507,.T.);
#3242=EDGE_CURVE('',#2683,#2682,#1508,.T.);
#3243=EDGE_CURVE('',#2684,#2683,#1509,.T.);
#3244=EDGE_CURVE('',#2684,#2681,#1510,.T.);
#3245=EDGE_CURVE('',#2675,#2685,#1511,.T.);
#3246=EDGE_CURVE('',#2682,#2685,#1512,.T.);
#3247=EDGE_CURVE('',#2681,#2679,#1513,.T.);
#3248=EDGE_CURVE('',#2686,#2683,#1514,.T.);
#3249=EDGE_CURVE('',#2676,#2686,#1515,.T.);
#3250=EDGE_CURVE('',#2680,#2684,#1516,.T.);
#3251=EDGE_CURVE('',#2685,#2686,#1517,.T.);
#3252=EDGE_CURVE('',#2687,#2687,#2341,.T.);
#3253=EDGE_CURVE('',#2687,#2688,#1518,.T.);
#3254=EDGE_CURVE('',#2688,#2688,#2342,.T.);
#3255=EDGE_CURVE('',#2689,#2689,#2343,.T.);
#3256=EDGE_CURVE('',#2689,#2690,#1519,.T.);
#3257=EDGE_CURVE('',#2690,#2690,#2344,.T.);
#3258=EDGE_CURVE('',#2691,#2691,#2345,.T.);
#3259=EDGE_CURVE('',#2691,#2692,#1520,.T.);
#3260=EDGE_CURVE('',#2692,#2692,#2346,.T.);
#3261=EDGE_CURVE('',#2693,#2693,#2347,.T.);
#3262=EDGE_CURVE('',#2693,#2694,#1521,.T.);
#3263=EDGE_CURVE('',#2694,#2694,#2348,.T.);
#3264=EDGE_CURVE('',#2695,#2695,#2349,.T.);
#3265=EDGE_CURVE('',#2695,#2696,#1522,.T.);
#3266=EDGE_CURVE('',#2696,#2696,#2350,.T.);
#3267=EDGE_CURVE('',#2697,#2697,#2351,.T.);
#3268=EDGE_CURVE('',#2697,#2698,#1523,.T.);
#3269=EDGE_CURVE('',#2698,#2698,#2352,.T.);
#3270=EDGE_CURVE('',#2699,#2699,#2353,.T.);
#3271=EDGE_CURVE('',#2699,#2700,#1524,.T.);
#3272=EDGE_CURVE('',#2700,#2700,#2354,.T.);
#3273=EDGE_CURVE('',#2701,#2701,#2355,.T.);
#3274=EDGE_CURVE('',#2701,#2702,#1525,.T.);
#3275=EDGE_CURVE('',#2702,#2702,#2356,.T.);
#3276=EDGE_CURVE('',#2703,#2704,#1526,.T.);
#3277=EDGE_CURVE('',#2704,#2705,#1527,.T.);
#3278=EDGE_CURVE('',#2706,#2705,#1528,.T.);
#3279=EDGE_CURVE('',#2703,#2706,#1529,.T.);
#3280=EDGE_CURVE('',#2707,#2703,#1530,.T.);
#3281=EDGE_CURVE('',#2708,#2706,#1531,.T.);
#3282=EDGE_CURVE('',#2707,#2708,#1532,.T.);
#3283=EDGE_CURVE('',#2709,#2707,#1533,.T.);
#3284=EDGE_CURVE('',#2710,#2708,#1534,.T.);
#3285=EDGE_CURVE('',#2709,#2710,#1535,.T.);
#3286=EDGE_CURVE('',#2704,#2709,#1536,.T.);
#3287=EDGE_CURVE('',#2705,#2710,#1537,.T.);
#3288=EDGE_CURVE('',#2711,#2712,#1538,.T.);
#3289=EDGE_CURVE('',#2712,#2713,#1539,.T.);
#3290=EDGE_CURVE('',#2714,#2713,#1540,.T.);
#3291=EDGE_CURVE('',#2711,#2714,#1541,.T.);
#3292=EDGE_CURVE('',#2715,#2711,#1542,.T.);
#3293=EDGE_CURVE('',#2716,#2714,#1543,.T.);
#3294=EDGE_CURVE('',#2715,#2716,#1544,.T.);
#3295=EDGE_CURVE('',#2717,#2715,#1545,.T.);
#3296=EDGE_CURVE('',#2718,#2716,#1546,.T.);
#3297=EDGE_CURVE('',#2717,#2718,#1547,.T.);
#3298=EDGE_CURVE('',#2712,#2717,#1548,.T.);
#3299=EDGE_CURVE('',#2713,#2718,#1549,.T.);
#3300=EDGE_CURVE('',#2719,#2720,#1550,.T.);
#3301=EDGE_CURVE('',#2720,#2721,#1551,.T.);
#3302=EDGE_CURVE('',#2721,#2722,#1552,.T.);
#3303=EDGE_CURVE('',#2719,#2722,#1553,.T.);
#3304=EDGE_CURVE('',#2720,#2723,#1554,.T.);
#3305=EDGE_CURVE('',#2723,#2724,#1555,.T.);
#3306=EDGE_CURVE('',#2724,#2721,#1556,.T.);
#3307=EDGE_CURVE('',#2723,#2725,#1557,.T.);
#3308=EDGE_CURVE('',#2725,#2726,#1558,.T.);
#3309=EDGE_CURVE('',#2726,#2724,#1559,.T.);
#3310=EDGE_CURVE('',#2725,#2727,#1560,.T.);
#3311=EDGE_CURVE('',#2727,#2728,#1561,.T.);
#3312=EDGE_CURVE('',#2728,#2726,#1562,.T.);
#3313=EDGE_CURVE('',#2727,#2729,#1563,.T.);
#3314=EDGE_CURVE('',#2729,#2730,#1564,.T.);
#3315=EDGE_CURVE('',#2730,#2728,#1565,.T.);
#3316=EDGE_CURVE('',#2729,#2719,#1566,.T.);
#3317=EDGE_CURVE('',#2722,#2730,#1567,.T.);
#3318=EDGE_CURVE('',#2731,#2731,#2357,.T.);
#3319=EDGE_CURVE('',#2732,#2732,#2358,.T.);
#3320=EDGE_CURVE('',#2733,#2733,#2359,.T.);
#3321=EDGE_CURVE('',#2733,#2732,#1568,.T.);
#3322=EDGE_CURVE('',#2734,#2734,#2360,.T.);
#3323=EDGE_CURVE('',#2734,#2733,#1569,.T.);
#3324=EDGE_CURVE('',#2735,#2735,#2361,.T.);
#3325=EDGE_CURVE('',#2735,#2734,#1570,.T.);
#3326=EDGE_CURVE('',#2736,#2736,#2362,.T.);
#3327=EDGE_CURVE('',#2737,#2737,#2363,.F.);
#3328=EDGE_CURVE('',#2737,#2736,#1571,.T.);
#3329=EDGE_CURVE('',#2731,#2737,#1572,.T.);
#3330=EDGE_CURVE('',#2738,#2738,#2364,.T.);
#3331=EDGE_CURVE('',#2738,#2739,#1573,.T.);
#3332=EDGE_CURVE('',#2739,#2739,#2365,.T.);
#3333=EDGE_CURVE('',#2740,#2740,#2366,.T.);
#3334=EDGE_CURVE('',#2740,#2741,#1574,.T.);
#3335=EDGE_CURVE('',#2741,#2741,#2367,.T.);
#3336=EDGE_CURVE('',#2742,#2743,#2368,.T.);
#3337=EDGE_CURVE('',#2744,#2744,#2369,.T.);
#3338=EDGE_CURVE('',#2744,#2745,#1575,.T.);
#3339=EDGE_CURVE('',#2745,#2745,#2370,.T.);
#3340=EDGE_CURVE('',#2746,#2746,#2371,.T.);
#3341=EDGE_CURVE('',#2746,#2747,#1576,.T.);
#3342=EDGE_CURVE('',#2747,#2747,#2372,.T.);
#3343=EDGE_CURVE('',#2748,#2748,#2373,.T.);
#3344=EDGE_CURVE('',#2748,#2749,#1577,.T.);
#3345=EDGE_CURVE('',#2749,#2749,#2374,.T.);
#3346=EDGE_CURVE('',#2750,#2750,#2375,.T.);
#3347=EDGE_CURVE('',#2750,#2751,#1578,.T.);
#3348=EDGE_CURVE('',#2751,#2751,#2376,.T.);
#3349=EDGE_CURVE('',#2752,#2752,#2377,.T.);
#3350=EDGE_CURVE('',#2752,#2753,#1579,.T.);
#3351=EDGE_CURVE('',#2753,#2753,#2378,.T.);
#3352=EDGE_CURVE('',#2754,#2754,#2379,.T.);
#3353=EDGE_CURVE('',#2754,#2755,#1580,.T.);
#3354=EDGE_CURVE('',#2755,#2755,#2380,.T.);
#3355=EDGE_CURVE('',#2756,#2757,#1581,.T.);
#3356=EDGE_CURVE('',#2757,#2758,#1582,.T.);
#3357=EDGE_CURVE('',#2759,#2758,#1583,.T.);
#3358=EDGE_CURVE('',#2756,#2759,#1584,.T.);
#3359=EDGE_CURVE('',#2760,#2756,#1585,.T.);
#3360=EDGE_CURVE('',#2761,#2759,#1586,.T.);
#3361=EDGE_CURVE('',#2760,#2761,#1587,.T.);
#3362=EDGE_CURVE('',#2762,#2760,#1588,.T.);
#3363=EDGE_CURVE('',#2763,#2761,#1589,.T.);
#3364=EDGE_CURVE('',#2762,#2763,#1590,.T.);
#3365=EDGE_CURVE('',#2764,#2762,#1591,.T.);
#3366=EDGE_CURVE('',#2765,#2763,#1592,.T.);
#3367=EDGE_CURVE('',#2764,#2765,#1593,.T.);
#3368=EDGE_CURVE('',#2766,#2764,#1594,.T.);
#3369=EDGE_CURVE('',#2767,#2765,#1595,.T.);
#3370=EDGE_CURVE('',#2766,#2767,#1596,.T.);
#3371=EDGE_CURVE('',#2768,#2766,#1597,.T.);
#3372=EDGE_CURVE('',#2769,#2767,#1598,.T.);
#3373=EDGE_CURVE('',#2768,#2769,#1599,.T.);
#3374=EDGE_CURVE('',#2770,#2768,#1600,.T.);
#3375=EDGE_CURVE('',#2771,#2769,#1601,.T.);
#3376=EDGE_CURVE('',#2770,#2771,#1602,.T.);
#3377=EDGE_CURVE('',#2757,#2770,#1603,.T.);
#3378=EDGE_CURVE('',#2758,#2771,#1604,.T.);
#3379=EDGE_CURVE('',#2772,#2772,#2381,.T.);
#3380=EDGE_CURVE('',#2772,#2773,#1605,.T.);
#3381=EDGE_CURVE('',#2773,#2773,#2382,.T.);
#3382=EDGE_CURVE('',#2774,#2774,#2383,.T.);
#3383=EDGE_CURVE('',#2775,#2776,#2384,.T.);
#3384=EDGE_CURVE('',#2777,#2777,#2385,.T.);
#3385=EDGE_CURVE('',#2778,#2779,#211,.T.);
#3386=EDGE_CURVE('',#2780,#2778,#212,.T.);
#3387=EDGE_CURVE('',#2779,#2780,#213,.T.);
#3388=EDGE_CURVE('',#2779,#2781,#1606,.T.);
#3389=EDGE_CURVE('',#2781,#2781,#214,.T.);
#3390=EDGE_CURVE('',#2782,#2782,#215,.T.);
#3391=EDGE_CURVE('',#2782,#2783,#1607,.T.);
#3392=EDGE_CURVE('',#2784,#2783,#216,.T.);
#3393=EDGE_CURVE('',#2785,#2784,#217,.T.);
#3394=EDGE_CURVE('',#2783,#2785,#218,.T.);
#3395=EDGE_CURVE('',#2786,#2786,#2386,.T.);
#3396=EDGE_CURVE('',#2786,#2787,#1608,.T.);
#3397=EDGE_CURVE('',#2787,#2787,#2387,.T.);
#3398=EDGE_CURVE('',#2788,#2789,#219,.T.);
#3399=EDGE_CURVE('',#2789,#2790,#220,.T.);
#3400=EDGE_CURVE('',#2790,#2788,#221,.T.);
#3401=EDGE_CURVE('',#2791,#2792,#222,.T.);
#3402=EDGE_CURVE('',#2792,#2793,#223,.T.);
#3403=EDGE_CURVE('',#2793,#2791,#224,.T.);
#3404=EDGE_CURVE('',#2794,#2795,#225,.T.);
#3405=EDGE_CURVE('',#2795,#2796,#226,.T.);
#3406=EDGE_CURVE('',#2796,#2794,#227,.T.);
#3407=EDGE_CURVE('',#2797,#2798,#228,.T.);
#3408=EDGE_CURVE('',#2798,#2799,#229,.T.);
#3409=EDGE_CURVE('',#2799,#2797,#230,.T.);
#3410=EDGE_CURVE('',#2790,#2800,#1609,.T.);
#3411=EDGE_CURVE('',#2800,#2800,#231,.T.);
#3412=EDGE_CURVE('',#2801,#2801,#232,.T.);
#3413=EDGE_CURVE('',#2801,#2793,#1610,.T.);
#3414=EDGE_CURVE('',#2796,#2802,#1611,.T.);
#3415=EDGE_CURVE('',#2802,#2802,#233,.T.);
#3416=EDGE_CURVE('',#2803,#2803,#234,.T.);
#3417=EDGE_CURVE('',#2803,#2799,#1612,.T.);
#3418=EDGE_CURVE('',#2804,#2804,#2388,.T.);
#3419=EDGE_CURVE('',#2805,#2805,#2389,.T.);
#3420=EDGE_CURVE('',#2806,#2806,#2390,.T.);
#3421=EDGE_CURVE('',#2806,#2805,#1613,.T.);
#3422=EDGE_CURVE('',#2807,#2807,#2391,.T.);
#3423=EDGE_CURVE('',#2807,#2804,#1614,.T.);
#3424=EDGE_CURVE('',#2808,#2808,#2392,.T.);
#3425=EDGE_CURVE('',#2809,#2809,#2393,.T.);
#3426=EDGE_CURVE('',#2809,#2808,#1615,.T.);
#3427=EDGE_CURVE('',#2810,#2810,#2394,.T.);
#3428=EDGE_CURVE('',#2810,#2809,#1616,.T.);
#3429=EDGE_CURVE('',#2811,#2811,#2395,.T.);
#3430=EDGE_CURVE('',#2811,#2810,#1617,.T.);
#3431=EDGE_CURVE('',#2812,#2812,#2396,.T.);
#3432=EDGE_CURVE('',#2813,#2813,#2397,.F.);
#3433=EDGE_CURVE('',#2813,#2812,#1618,.T.);
#3434=EDGE_CURVE('',#2814,#2814,#2398,.F.);
#3435=EDGE_CURVE('',#2814,#2813,#1619,.T.);
#3436=EDGE_CURVE('',#2815,#2815,#2399,.T.);
#3437=EDGE_CURVE('',#2815,#2814,#1620,.T.);
#3438=EDGE_CURVE('',#2816,#2817,#1621,.T.);
#3439=EDGE_CURVE('',#2817,#2818,#1622,.T.);
#3440=EDGE_CURVE('',#2818,#2819,#1623,.T.);
#3441=EDGE_CURVE('',#2816,#2819,#1624,.T.);
#3442=EDGE_CURVE('',#2817,#2820,#1625,.T.);
#3443=EDGE_CURVE('',#2820,#2821,#1626,.T.);
#3444=EDGE_CURVE('',#2821,#2818,#1627,.T.);
#3445=EDGE_CURVE('',#2820,#2822,#1628,.T.);
#3446=EDGE_CURVE('',#2822,#2823,#1629,.T.);
#3447=EDGE_CURVE('',#2823,#2821,#1630,.T.);
#3448=EDGE_CURVE('',#2822,#2824,#1631,.T.);
#3449=EDGE_CURVE('',#2824,#2825,#1632,.T.);
#3450=EDGE_CURVE('',#2825,#2823,#1633,.T.);
#3451=EDGE_CURVE('',#2824,#2826,#1634,.T.);
#3452=EDGE_CURVE('',#2826,#2827,#1635,.T.);
#3453=EDGE_CURVE('',#2827,#2825,#1636,.T.);
#3454=EDGE_CURVE('',#2826,#2816,#1637,.T.);
#3455=EDGE_CURVE('',#2819,#2827,#1638,.T.);
#3456=EDGE_CURVE('',#2828,#2829,#1639,.T.);
#3457=EDGE_CURVE('',#2828,#2830,#1640,.T.);
#3458=EDGE_CURVE('',#2831,#2830,#1641,.T.);
#3459=EDGE_CURVE('',#2831,#2829,#1642,.T.);
#3460=EDGE_CURVE('',#2829,#2832,#2400,.T.);
#3461=EDGE_CURVE('',#2833,#2831,#1643,.T.);
#3462=EDGE_CURVE('',#2832,#2833,#1644,.T.);
#3463=EDGE_CURVE('',#2832,#2834,#1645,.T.);
#3464=EDGE_CURVE('',#2833,#2835,#1646,.T.);
#3465=EDGE_CURVE('',#2835,#2834,#1647,.T.);
#3466=EDGE_CURVE('',#2830,#2835,#1648,.T.);
#3467=EDGE_CURVE('',#2834,#2828,#2401,.T.);
#3468=EDGE_CURVE('',#2836,#2836,#2402,.T.);
#3469=EDGE_CURVE('',#2836,#2837,#1649,.T.);
#3470=EDGE_CURVE('',#2837,#2837,#2403,.T.);
#3471=EDGE_CURVE('',#2838,#2839,#1650,.T.);
#3472=EDGE_CURVE('',#2838,#2840,#1651,.T.);
#3473=EDGE_CURVE('',#2841,#2840,#1652,.T.);
#3474=EDGE_CURVE('',#2841,#2839,#1653,.T.);
#3475=EDGE_CURVE('',#2839,#2842,#2404,.T.);
#3476=EDGE_CURVE('',#2843,#2841,#1654,.T.);
#3477=EDGE_CURVE('',#2842,#2843,#1655,.T.);
#3478=EDGE_CURVE('',#2842,#2844,#1656,.T.);
#3479=EDGE_CURVE('',#2843,#2845,#1657,.T.);
#3480=EDGE_CURVE('',#2845,#2844,#1658,.T.);
#3481=EDGE_CURVE('',#2840,#2845,#1659,.T.);
#3482=EDGE_CURVE('',#2844,#2838,#2405,.T.);
#3483=EDGE_CURVE('',#2846,#2846,#2406,.T.);
#3484=EDGE_CURVE('',#2846,#2847,#1660,.T.);
#3485=EDGE_CURVE('',#2847,#2847,#2407,.T.);
#3486=EDGE_CURVE('',#2848,#2848,#2408,.T.);
#3487=EDGE_CURVE('',#2848,#2849,#1661,.T.);
#3488=EDGE_CURVE('',#2849,#2849,#2409,.T.);
#3489=EDGE_CURVE('',#2850,#2850,#2410,.T.);
#3490=EDGE_CURVE('',#2850,#2851,#1662,.T.);
#3491=EDGE_CURVE('',#2851,#2851,#2411,.T.);
#3492=EDGE_CURVE('',#2852,#2852,#2412,.T.);
#3493=EDGE_CURVE('',#2852,#2853,#1663,.T.);
#3494=EDGE_CURVE('',#2853,#2853,#2413,.T.);
#3495=EDGE_CURVE('',#2854,#2854,#2414,.T.);
#3496=EDGE_CURVE('',#2854,#2855,#1664,.T.);
#3497=EDGE_CURVE('',#2855,#2855,#2415,.T.);
#3498=EDGE_CURVE('',#2856,#2856,#2416,.T.);
#3499=EDGE_CURVE('',#2856,#2857,#1665,.T.);
#3500=EDGE_CURVE('',#2857,#2857,#2417,.T.);
#3501=EDGE_CURVE('',#2858,#2858,#2418,.T.);
#3502=EDGE_CURVE('',#2858,#2859,#1666,.T.);
#3503=EDGE_CURVE('',#2859,#2859,#2419,.T.);
#3504=EDGE_CURVE('',#2860,#2860,#2420,.T.);
#3505=EDGE_CURVE('',#2860,#2861,#1667,.T.);
#3506=EDGE_CURVE('',#2861,#2861,#2421,.T.);
#3507=EDGE_CURVE('',#2862,#2862,#2422,.T.);
#3508=EDGE_CURVE('',#2862,#2863,#1668,.T.);
#3509=EDGE_CURVE('',#2863,#2863,#2423,.T.);
#3510=EDGE_CURVE('',#2864,#2865,#1669,.T.);
#3511=EDGE_CURVE('',#2864,#2865,#2424,.T.);
#3512=EDGE_CURVE('',#2866,#2864,#235,.T.);
#3513=EDGE_CURVE('',#2867,#2866,#2425,.T.);
#3514=EDGE_CURVE('',#2867,#2868,#1670,.T.);
#3515=EDGE_CURVE('',#2869,#2868,#236,.T.);
#3516=EDGE_CURVE('',#2868,#2869,#237,.T.);
#3517=EDGE_CURVE('',#2870,#2867,#2426,.T.);
#3518=EDGE_CURVE('',#2865,#2870,#238,.T.);
#3519=EDGE_CURVE('',#2870,#2866,#1671,.T.);
#3520=EDGE_CURVE('',#2871,#2871,#2427,.T.);
#3521=EDGE_CURVE('',#2871,#2872,#1672,.T.);
#3522=EDGE_CURVE('',#2872,#2872,#2428,.T.);
#3523=EDGE_CURVE('',#2873,#2873,#2429,.T.);
#3524=EDGE_CURVE('',#2873,#2874,#1673,.T.);
#3525=EDGE_CURVE('',#2874,#2874,#2430,.T.);
#3526=EDGE_CURVE('',#2875,#2876,#1674,.T.);
#3527=EDGE_CURVE('',#2875,#2876,#2431,.T.);
#3528=EDGE_CURVE('',#2877,#2875,#239,.T.);
#3529=EDGE_CURVE('',#2878,#2877,#2432,.T.);
#3530=EDGE_CURVE('',#2878,#2879,#1675,.T.);
#3531=EDGE_CURVE('',#2880,#2879,#240,.T.);
#3532=EDGE_CURVE('',#2879,#2880,#241,.T.);
#3533=EDGE_CURVE('',#2881,#2878,#2433,.T.);
#3534=EDGE_CURVE('',#2876,#2881,#242,.T.);
#3535=EDGE_CURVE('',#2881,#2877,#1676,.T.);
#3536=EDGE_CURVE('',#2882,#2882,#2434,.T.);
#3537=EDGE_CURVE('',#2882,#2883,#1677,.T.);
#3538=EDGE_CURVE('',#2883,#2883,#2435,.T.);
#3539=EDGE_CURVE('',#2884,#2884,#2436,.T.);
#3540=EDGE_CURVE('',#2884,#2885,#1678,.T.);
#3541=EDGE_CURVE('',#2885,#2885,#2437,.T.);
#3542=EDGE_CURVE('',#2886,#2887,#1679,.T.);
#3543=EDGE_CURVE('',#2886,#2888,#1680,.T.);
#3544=EDGE_CURVE('',#2889,#2888,#1681,.T.);
#3545=EDGE_CURVE('',#2887,#2889,#1682,.T.);
#3546=EDGE_CURVE('',#2890,#2886,#1683,.T.);
#3547=EDGE_CURVE('',#2890,#2891,#1684,.T.);
#3548=EDGE_CURVE('',#2888,#2891,#1685,.T.);
#3549=EDGE_CURVE('',#2892,#2890,#1686,.T.);
#3550=EDGE_CURVE('',#2893,#2892,#1687,.T.);
#3551=EDGE_CURVE('',#2891,#2893,#1688,.T.);
#3552=EDGE_CURVE('',#2894,#2894,#2438,.T.);
#3553=EDGE_CURVE('',#2895,#2895,#2439,.T.);
#3554=EDGE_CURVE('',#2896,#2896,#2440,.T.);
#3555=EDGE_CURVE('',#2897,#2897,#2441,.T.);
#3556=EDGE_CURVE('',#2898,#2898,#2442,.T.);
#3557=EDGE_CURVE('',#2899,#2899,#2443,.T.);
#3558=EDGE_CURVE('',#2900,#2900,#2444,.T.);
#3559=EDGE_CURVE('',#2893,#2889,#2445,.T.);
#3560=EDGE_CURVE('',#2892,#2887,#2446,.T.);
#3561=EDGE_CURVE('',#2901,#2901,#2447,.T.);
#3562=EDGE_CURVE('',#2901,#2895,#1689,.T.);
#3563=EDGE_CURVE('',#2902,#2902,#2448,.T.);
#3564=EDGE_CURVE('',#2902,#2896,#1690,.T.);
#3565=EDGE_CURVE('',#2903,#2903,#2449,.T.);
#3566=EDGE_CURVE('',#2903,#2897,#1691,.T.);
#3567=EDGE_CURVE('',#2904,#2904,#2450,.T.);
#3568=EDGE_CURVE('',#2904,#2898,#1692,.T.);
#3569=EDGE_CURVE('',#2905,#2905,#2451,.T.);
#3570=EDGE_CURVE('',#2905,#2899,#1693,.T.);
#3571=EDGE_CURVE('',#2906,#2906,#2452,.T.);
#3572=EDGE_CURVE('',#2906,#2900,#1694,.T.);
#3573=EDGE_CURVE('',#2907,#2907,#2453,.T.);
#3574=EDGE_CURVE('',#2908,#2908,#2454,.T.);
#3575=EDGE_CURVE('',#2894,#2907,#1695,.T.);
#3576=EDGE_CURVE('',#2908,#2909,#1696,.T.);
#3577=EDGE_CURVE('',#2909,#2909,#2455,.T.);
#3578=EDGE_CURVE('',#2910,#2910,#2456,.T.);
#3579=EDGE_CURVE('',#2910,#2911,#1697,.T.);
#3580=EDGE_CURVE('',#2911,#2911,#2457,.T.);
#3581=EDGE_CURVE('',#2912,#2912,#2458,.T.);
#3582=EDGE_CURVE('',#2912,#2913,#1698,.T.);
#3583=EDGE_CURVE('',#2913,#2913,#2459,.T.);
#3584=EDGE_CURVE('',#2914,#2915,#1699,.T.);
#3585=EDGE_CURVE('',#2914,#2916,#1700,.T.);
#3586=EDGE_CURVE('',#2917,#2916,#1701,.T.);
#3587=EDGE_CURVE('',#2915,#2917,#1702,.T.);
#3588=EDGE_CURVE('',#2918,#2914,#1703,.T.);
#3589=EDGE_CURVE('',#2918,#2919,#1704,.T.);
#3590=EDGE_CURVE('',#2916,#2919,#1705,.T.);
#3591=EDGE_CURVE('',#2920,#2920,#2460,.T.);
#3592=EDGE_CURVE('',#2921,#2918,#1706,.T.);
#3593=EDGE_CURVE('',#2922,#2921,#1707,.T.);
#3594=EDGE_CURVE('',#2919,#2922,#1708,.T.);
#3595=EDGE_CURVE('',#2923,#2923,#2461,.T.);
#3596=EDGE_CURVE('',#2922,#2917,#2462,.T.);
#3597=EDGE_CURVE('',#2915,#2921,#2463,.T.);
#3598=EDGE_CURVE('',#2924,#2925,#243,.T.);
#3599=EDGE_CURVE('',#2925,#2924,#244,.T.);
#3600=EDGE_CURVE('',#2926,#2927,#245,.T.);
#3601=EDGE_CURVE('',#2927,#2926,#246,.T.);
#3602=EDGE_CURVE('',#2928,#2929,#247,.T.);
#3603=EDGE_CURVE('',#2929,#2928,#248,.T.);
#3604=EDGE_CURVE('',#2930,#2931,#249,.T.);
#3605=EDGE_CURVE('',#2932,#2930,#250,.T.);
#3606=EDGE_CURVE('',#2931,#2932,#251,.T.);
#3607=EDGE_CURVE('',#2931,#2927,#1709,.T.);
#3608=EDGE_CURVE('',#2929,#2933,#1710,.T.);
#3609=EDGE_CURVE('',#2934,#2933,#252,.T.);
#3610=EDGE_CURVE('',#2935,#2934,#253,.T.);
#3611=EDGE_CURVE('',#2933,#2935,#254,.T.);
#3612=EDGE_CURVE('',#2936,#2936,#2464,.T.);
#3613=EDGE_CURVE('',#2936,#2932,#1711,.T.);
#3614=EDGE_CURVE('',#2930,#2937,#1712,.T.);
#3615=EDGE_CURVE('',#2937,#2937,#2465,.T.);
#3616=EDGE_CURVE('',#2938,#2939,#255,.T.);
#3617=EDGE_CURVE('',#2939,#2940,#256,.T.);
#3618=EDGE_CURVE('',#2940,#2938,#257,.T.);
#3619=EDGE_CURVE('',#2941,#2942,#258,.T.);
#3620=EDGE_CURVE('',#2942,#2943,#259,.T.);
#3621=EDGE_CURVE('',#2943,#2941,#260,.T.);
#3622=EDGE_CURVE('',#2940,#2920,#1713,.T.);
#3623=EDGE_CURVE('',#2925,#2943,#1714,.T.);
#3624=EDGE_CURVE('',#2944,#2944,#2466,.T.);
#3625=EDGE_CURVE('',#2945,#2946,#2467,.T.);
#3626=EDGE_CURVE('',#2947,#2946,#2468,.T.);
#3627=EDGE_CURVE('',#2947,#2948,#2469,.T.);
#3628=EDGE_CURVE('',#2949,#2948,#2470,.T.);
#3629=EDGE_CURVE('',#2949,#2950,#2471,.T.);
#3630=EDGE_CURVE('',#2951,#2950,#2472,.T.);
#3631=EDGE_CURVE('',#2951,#2952,#2473,.T.);
#3632=EDGE_CURVE('',#2953,#2952,#2474,.T.);
#3633=EDGE_CURVE('',#2953,#2954,#2475,.T.);
#3634=EDGE_CURVE('',#2955,#2954,#2476,.T.);
#3635=EDGE_CURVE('',#2955,#2956,#2477,.T.);
#3636=EDGE_CURVE('',#2957,#2956,#2478,.T.);
#3637=EDGE_CURVE('',#2957,#2958,#2479,.T.);
#3638=EDGE_CURVE('',#2959,#2958,#2480,.T.);
#3639=EDGE_CURVE('',#2959,#2960,#2481,.T.);
#3640=EDGE_CURVE('',#2961,#2960,#2482,.T.);
#3641=EDGE_CURVE('',#2961,#2962,#2483,.T.);
#3642=EDGE_CURVE('',#2963,#2962,#2484,.T.);
#3643=EDGE_CURVE('',#2963,#2964,#2485,.T.);
#3644=EDGE_CURVE('',#2965,#2964,#2486,.T.);
#3645=EDGE_CURVE('',#2965,#2966,#2487,.T.);
#3646=EDGE_CURVE('',#2967,#2966,#2488,.T.);
#3647=EDGE_CURVE('',#2967,#2968,#2489,.T.);
#3648=EDGE_CURVE('',#2969,#2968,#2490,.T.);
#3649=EDGE_CURVE('',#2969,#2970,#2491,.T.);
#3650=EDGE_CURVE('',#2971,#2970,#2492,.T.);
#3651=EDGE_CURVE('',#2971,#2972,#2493,.T.);
#3652=EDGE_CURVE('',#2973,#2972,#2494,.T.);
#3653=EDGE_CURVE('',#2973,#2974,#2495,.T.);
#3654=EDGE_CURVE('',#2975,#2974,#2496,.T.);
#3655=EDGE_CURVE('',#2975,#2976,#2497,.T.);
#3656=EDGE_CURVE('',#2977,#2976,#2498,.T.);
#3657=EDGE_CURVE('',#2977,#2978,#2499,.T.);
#3658=EDGE_CURVE('',#2979,#2978,#2500,.T.);
#3659=EDGE_CURVE('',#2979,#2980,#2501,.T.);
#3660=EDGE_CURVE('',#2981,#2980,#2502,.T.);
#3661=EDGE_CURVE('',#2981,#2982,#2503,.T.);
#3662=EDGE_CURVE('',#2983,#2982,#2504,.T.);
#3663=EDGE_CURVE('',#2983,#2984,#2505,.T.);
#3664=EDGE_CURVE('',#2985,#2984,#2506,.T.);
#3665=EDGE_CURVE('',#2985,#2986,#2507,.T.);
#3666=EDGE_CURVE('',#2987,#2986,#2508,.T.);
#3667=EDGE_CURVE('',#2987,#2988,#2509,.T.);
#3668=EDGE_CURVE('',#2989,#2988,#2510,.T.);
#3669=EDGE_CURVE('',#2989,#2990,#2511,.T.);
#3670=EDGE_CURVE('',#2991,#2990,#2512,.T.);
#3671=EDGE_CURVE('',#2991,#2992,#2513,.T.);
#3672=EDGE_CURVE('',#2993,#2992,#2514,.T.);
#3673=EDGE_CURVE('',#2993,#2994,#2515,.T.);
#3674=EDGE_CURVE('',#2995,#2994,#2516,.T.);
#3675=EDGE_CURVE('',#2995,#2996,#2517,.T.);
#3676=EDGE_CURVE('',#2997,#2996,#2518,.T.);
#3677=EDGE_CURVE('',#2997,#2998,#2519,.T.);
#3678=EDGE_CURVE('',#2999,#2998,#2520,.T.);
#3679=EDGE_CURVE('',#2999,#3000,#2521,.T.);
#3680=EDGE_CURVE('',#3001,#3000,#2522,.T.);
#3681=EDGE_CURVE('',#3001,#3002,#2523,.T.);
#3682=EDGE_CURVE('',#3003,#3002,#2524,.T.);
#3683=EDGE_CURVE('',#3003,#3004,#2525,.T.);
#3684=EDGE_CURVE('',#3005,#3004,#2526,.T.);
#3685=EDGE_CURVE('',#3005,#3006,#2527,.T.);
#3686=EDGE_CURVE('',#3007,#3006,#2528,.T.);
#3687=EDGE_CURVE('',#3007,#3008,#2529,.T.);
#3688=EDGE_CURVE('',#3009,#3008,#2530,.T.);
#3689=EDGE_CURVE('',#3009,#3010,#2531,.T.);
#3690=EDGE_CURVE('',#3011,#3010,#2532,.T.);
#3691=EDGE_CURVE('',#3011,#3012,#2533,.T.);
#3692=EDGE_CURVE('',#3013,#3012,#2534,.T.);
#3693=EDGE_CURVE('',#3013,#3014,#2535,.T.);
#3694=EDGE_CURVE('',#3015,#3014,#2536,.T.);
#3695=EDGE_CURVE('',#3015,#3016,#2537,.T.);
#3696=EDGE_CURVE('',#3017,#3016,#2538,.T.);
#3697=EDGE_CURVE('',#3017,#3018,#2539,.T.);
#3698=EDGE_CURVE('',#3019,#3018,#2540,.T.);
#3699=EDGE_CURVE('',#3019,#3020,#2541,.T.);
#3700=EDGE_CURVE('',#3021,#3020,#2542,.T.);
#3701=EDGE_CURVE('',#3021,#3022,#2543,.T.);
#3702=EDGE_CURVE('',#3023,#3022,#2544,.T.);
#3703=EDGE_CURVE('',#3023,#3024,#2545,.T.);
#3704=EDGE_CURVE('',#2945,#3024,#2546,.T.);
#3705=EDGE_CURVE('',#3025,#3025,#2547,.T.);
#3706=EDGE_CURVE('',#3025,#2944,#1715,.T.);
#3707=EDGE_CURVE('',#3026,#3026,#2548,.T.);
#3708=EDGE_CURVE('',#3027,#3028,#2549,.T.);
#3709=EDGE_CURVE('',#3028,#3029,#2550,.T.);
#3710=EDGE_CURVE('',#3029,#3030,#2551,.T.);
#3711=EDGE_CURVE('',#3030,#3031,#2552,.T.);
#3712=EDGE_CURVE('',#3031,#3032,#2553,.T.);
#3713=EDGE_CURVE('',#3032,#3033,#2554,.T.);
#3714=EDGE_CURVE('',#3033,#3034,#2555,.T.);
#3715=EDGE_CURVE('',#3034,#3035,#2556,.T.);
#3716=EDGE_CURVE('',#3035,#3036,#2557,.T.);
#3717=EDGE_CURVE('',#3036,#3037,#2558,.T.);
#3718=EDGE_CURVE('',#3037,#3038,#2559,.T.);
#3719=EDGE_CURVE('',#3038,#3039,#2560,.T.);
#3720=EDGE_CURVE('',#3039,#3040,#2561,.T.);
#3721=EDGE_CURVE('',#3040,#3041,#2562,.T.);
#3722=EDGE_CURVE('',#3041,#3042,#2563,.T.);
#3723=EDGE_CURVE('',#3042,#3043,#2564,.T.);
#3724=EDGE_CURVE('',#3043,#3044,#2565,.T.);
#3725=EDGE_CURVE('',#3044,#3045,#2566,.T.);
#3726=EDGE_CURVE('',#3045,#3046,#2567,.T.);
#3727=EDGE_CURVE('',#3046,#3047,#2568,.T.);
#3728=EDGE_CURVE('',#3047,#3048,#2569,.T.);
#3729=EDGE_CURVE('',#3048,#3049,#2570,.T.);
#3730=EDGE_CURVE('',#3049,#3050,#2571,.T.);
#3731=EDGE_CURVE('',#3050,#3051,#2572,.T.);
#3732=EDGE_CURVE('',#3051,#3052,#2573,.T.);
#3733=EDGE_CURVE('',#3052,#3053,#2574,.T.);
#3734=EDGE_CURVE('',#3053,#3054,#2575,.T.);
#3735=EDGE_CURVE('',#3054,#3055,#2576,.T.);
#3736=EDGE_CURVE('',#3055,#3056,#2577,.T.);
#3737=EDGE_CURVE('',#3056,#3057,#2578,.T.);
#3738=EDGE_CURVE('',#3057,#3058,#2579,.T.);
#3739=EDGE_CURVE('',#3058,#3059,#2580,.T.);
#3740=EDGE_CURVE('',#3059,#3060,#2581,.T.);
#3741=EDGE_CURVE('',#3060,#3061,#2582,.T.);
#3742=EDGE_CURVE('',#3061,#3062,#2583,.T.);
#3743=EDGE_CURVE('',#3062,#3063,#2584,.T.);
#3744=EDGE_CURVE('',#3063,#3064,#2585,.T.);
#3745=EDGE_CURVE('',#3064,#3065,#2586,.T.);
#3746=EDGE_CURVE('',#3065,#3066,#2587,.T.);
#3747=EDGE_CURVE('',#3066,#3067,#2588,.T.);
#3748=EDGE_CURVE('',#3067,#3068,#2589,.T.);
#3749=EDGE_CURVE('',#3068,#3069,#2590,.T.);
#3750=EDGE_CURVE('',#3069,#3070,#2591,.T.);
#3751=EDGE_CURVE('',#3070,#3071,#2592,.T.);
#3752=EDGE_CURVE('',#3071,#3072,#2593,.T.);
#3753=EDGE_CURVE('',#3072,#3073,#2594,.T.);
#3754=EDGE_CURVE('',#3073,#3074,#2595,.T.);
#3755=EDGE_CURVE('',#3074,#3075,#2596,.T.);
#3756=EDGE_CURVE('',#3075,#3076,#2597,.T.);
#3757=EDGE_CURVE('',#3076,#3077,#2598,.T.);
#3758=EDGE_CURVE('',#3077,#3078,#2599,.T.);
#3759=EDGE_CURVE('',#3078,#3079,#2600,.T.);
#3760=EDGE_CURVE('',#3079,#3080,#2601,.T.);
#3761=EDGE_CURVE('',#3080,#3081,#2602,.T.);
#3762=EDGE_CURVE('',#3081,#3082,#2603,.T.);
#3763=EDGE_CURVE('',#3082,#3083,#2604,.T.);
#3764=EDGE_CURVE('',#3083,#3084,#2605,.T.);
#3765=EDGE_CURVE('',#3084,#3085,#2606,.T.);
#3766=EDGE_CURVE('',#3085,#3086,#2607,.T.);
#3767=EDGE_CURVE('',#3086,#3087,#2608,.T.);
#3768=EDGE_CURVE('',#3087,#3088,#2609,.T.);
#3769=EDGE_CURVE('',#3088,#3089,#2610,.T.);
#3770=EDGE_CURVE('',#3089,#3090,#2611,.T.);
#3771=EDGE_CURVE('',#3090,#3091,#2612,.T.);
#3772=EDGE_CURVE('',#3091,#3092,#2613,.T.);
#3773=EDGE_CURVE('',#3092,#3093,#2614,.T.);
#3774=EDGE_CURVE('',#3093,#3094,#2615,.T.);
#3775=EDGE_CURVE('',#3094,#3095,#2616,.T.);
#3776=EDGE_CURVE('',#3095,#3096,#2617,.T.);
#3777=EDGE_CURVE('',#3096,#3097,#2618,.T.);
#3778=EDGE_CURVE('',#3097,#3098,#2619,.T.);
#3779=EDGE_CURVE('',#3098,#3099,#2620,.T.);
#3780=EDGE_CURVE('',#3099,#3100,#2621,.T.);
#3781=EDGE_CURVE('',#3100,#3101,#2622,.T.);
#3782=EDGE_CURVE('',#3101,#3102,#2623,.T.);
#3783=EDGE_CURVE('',#3102,#3103,#2624,.T.);
#3784=EDGE_CURVE('',#3103,#3104,#2625,.T.);
#3785=EDGE_CURVE('',#3104,#3105,#2626,.T.);
#3786=EDGE_CURVE('',#3105,#3106,#2627,.T.);
#3787=EDGE_CURVE('',#3106,#3027,#2628,.T.);
#3788=EDGE_CURVE('',#2923,#3026,#1716,.T.);
#3789=EDGE_CURVE('',#3028,#2945,#1717,.T.);
#3790=EDGE_CURVE('',#2946,#3027,#1718,.T.);
#3791=EDGE_CURVE('',#3106,#2947,#1719,.T.);
#3792=EDGE_CURVE('',#2948,#3105,#1720,.T.);
#3793=EDGE_CURVE('',#3104,#2949,#1721,.T.);
#3794=EDGE_CURVE('',#2950,#3103,#1722,.T.);
#3795=EDGE_CURVE('',#3102,#2951,#1723,.T.);
#3796=EDGE_CURVE('',#2952,#3101,#1724,.T.);
#3797=EDGE_CURVE('',#3100,#2953,#1725,.T.);
#3798=EDGE_CURVE('',#2954,#3099,#1726,.T.);
#3799=EDGE_CURVE('',#3098,#2955,#1727,.T.);
#3800=EDGE_CURVE('',#2956,#3097,#1728,.T.);
#3801=EDGE_CURVE('',#3096,#2957,#1729,.T.);
#3802=EDGE_CURVE('',#2958,#3095,#1730,.T.);
#3803=EDGE_CURVE('',#3094,#2959,#1731,.T.);
#3804=EDGE_CURVE('',#2960,#3093,#1732,.T.);
#3805=EDGE_CURVE('',#3092,#2961,#1733,.T.);
#3806=EDGE_CURVE('',#2962,#3091,#1734,.T.);
#3807=EDGE_CURVE('',#3090,#2963,#1735,.T.);
#3808=EDGE_CURVE('',#2964,#3089,#1736,.T.);
#3809=EDGE_CURVE('',#3088,#2965,#1737,.T.);
#3810=EDGE_CURVE('',#2966,#3087,#1738,.T.);
#3811=EDGE_CURVE('',#3086,#2967,#1739,.T.);
#3812=EDGE_CURVE('',#2968,#3085,#1740,.T.);
#3813=EDGE_CURVE('',#3084,#2969,#1741,.T.);
#3814=EDGE_CURVE('',#2970,#3083,#1742,.T.);
#3815=EDGE_CURVE('',#3082,#2971,#1743,.T.);
#3816=EDGE_CURVE('',#2972,#3081,#1744,.T.);
#3817=EDGE_CURVE('',#3080,#2973,#1745,.T.);
#3818=EDGE_CURVE('',#2974,#3079,#1746,.T.);
#3819=EDGE_CURVE('',#3078,#2975,#1747,.T.);
#3820=EDGE_CURVE('',#2976,#3077,#1748,.T.);
#3821=EDGE_CURVE('',#3076,#2977,#1749,.T.);
#3822=EDGE_CURVE('',#2978,#3075,#1750,.T.);
#3823=EDGE_CURVE('',#3074,#2979,#1751,.T.);
#3824=EDGE_CURVE('',#2980,#3073,#1752,.T.);
#3825=EDGE_CURVE('',#3072,#2981,#1753,.T.);
#3826=EDGE_CURVE('',#2982,#3071,#1754,.T.);
#3827=EDGE_CURVE('',#3070,#2983,#1755,.T.);
#3828=EDGE_CURVE('',#2984,#3069,#1756,.T.);
#3829=EDGE_CURVE('',#3068,#2985,#1757,.T.);
#3830=EDGE_CURVE('',#2986,#3067,#1758,.T.);
#3831=EDGE_CURVE('',#3066,#2987,#1759,.T.);
#3832=EDGE_CURVE('',#2988,#3065,#1760,.T.);
#3833=EDGE_CURVE('',#3064,#2989,#1761,.T.);
#3834=EDGE_CURVE('',#2990,#3063,#1762,.T.);
#3835=EDGE_CURVE('',#3062,#2991,#1763,.T.);
#3836=EDGE_CURVE('',#2992,#3061,#1764,.T.);
#3837=EDGE_CURVE('',#3060,#2993,#1765,.T.);
#3838=EDGE_CURVE('',#2994,#3059,#1766,.T.);
#3839=EDGE_CURVE('',#3058,#2995,#1767,.T.);
#3840=EDGE_CURVE('',#2996,#3057,#1768,.T.);
#3841=EDGE_CURVE('',#3056,#2997,#1769,.T.);
#3842=EDGE_CURVE('',#2998,#3055,#1770,.T.);
#3843=EDGE_CURVE('',#3054,#2999,#1771,.T.);
#3844=EDGE_CURVE('',#3000,#3053,#1772,.T.);
#3845=EDGE_CURVE('',#3052,#3001,#1773,.T.);
#3846=EDGE_CURVE('',#3002,#3051,#1774,.T.);
#3847=EDGE_CURVE('',#3050,#3003,#1775,.T.);
#3848=EDGE_CURVE('',#3004,#3049,#1776,.T.);
#3849=EDGE_CURVE('',#3048,#3005,#1777,.T.);
#3850=EDGE_CURVE('',#3006,#3047,#1778,.T.);
#3851=EDGE_CURVE('',#3046,#3007,#1779,.T.);
#3852=EDGE_CURVE('',#3008,#3045,#1780,.T.);
#3853=EDGE_CURVE('',#3044,#3009,#1781,.T.);
#3854=EDGE_CURVE('',#3010,#3043,#1782,.T.);
#3855=EDGE_CURVE('',#3042,#3011,#1783,.T.);
#3856=EDGE_CURVE('',#3012,#3041,#1784,.T.);
#3857=EDGE_CURVE('',#3040,#3013,#1785,.T.);
#3858=EDGE_CURVE('',#3014,#3039,#1786,.T.);
#3859=EDGE_CURVE('',#3038,#3015,#1787,.T.);
#3860=EDGE_CURVE('',#3016,#3037,#1788,.T.);
#3861=EDGE_CURVE('',#3036,#3017,#1789,.T.);
#3862=EDGE_CURVE('',#3018,#3035,#1790,.T.);
#3863=EDGE_CURVE('',#3034,#3019,#1791,.T.);
#3864=EDGE_CURVE('',#3020,#3033,#1792,.T.);
#3865=EDGE_CURVE('',#3032,#3021,#1793,.T.);
#3866=EDGE_CURVE('',#3022,#3031,#1794,.T.);
#3867=EDGE_CURVE('',#3024,#3029,#1795,.T.);
#3868=EDGE_CURVE('',#3030,#3023,#1796,.T.);
#3869=EDGE_CURVE('',#3107,#3108,#1797,.T.);
#3870=EDGE_CURVE('',#3109,#3107,#1798,.T.);
#3871=EDGE_CURVE('',#3110,#3109,#1799,.T.);
#3872=EDGE_CURVE('',#3111,#3110,#1800,.T.);
#3873=EDGE_CURVE('',#3112,#3111,#1801,.T.);
#3874=EDGE_CURVE('',#3113,#3112,#1802,.T.);
#3875=EDGE_CURVE('',#3114,#3113,#1803,.T.);
#3876=EDGE_CURVE('',#3108,#3114,#1804,.T.);
#3877=EDGE_CURVE('',#3111,#3115,#1805,.T.);
#3878=EDGE_CURVE('',#3115,#3116,#1806,.T.);
#3879=EDGE_CURVE('',#3116,#3112,#1807,.T.);
#3880=EDGE_CURVE('',#3117,#3110,#1808,.T.);
#3881=EDGE_CURVE('',#3117,#3115,#1809,.T.);
#3882=EDGE_CURVE('',#3109,#3118,#1810,.T.);
#3883=EDGE_CURVE('',#3118,#3117,#1811,.T.);
#3884=EDGE_CURVE('',#3119,#3107,#1812,.T.);
#3885=EDGE_CURVE('',#3119,#3118,#1813,.T.);
#3886=EDGE_CURVE('',#3120,#3119,#1814,.T.);
#3887=EDGE_CURVE('',#3121,#3120,#1815,.T.);
#3888=EDGE_CURVE('',#3122,#3121,#1816,.T.);
#3889=EDGE_CURVE('',#3116,#3122,#1817,.T.);
#3890=EDGE_CURVE('',#3108,#3120,#1818,.T.);
#3891=EDGE_CURVE('',#3121,#3114,#1819,.T.);
#3892=EDGE_CURVE('',#3113,#3122,#1820,.T.);
#3893=EDGE_CURVE('',#3123,#3123,#2629,.T.);
#3894=EDGE_CURVE('',#3124,#3124,#2630,.T.);
#3895=EDGE_CURVE('',#3124,#3123,#1821,.T.);
#3896=EDGE_CURVE('',#3125,#3125,#2631,.T.);
#3897=EDGE_CURVE('',#3125,#3124,#1822,.T.);
#3898=EDGE_CURVE('',#3126,#3126,#2632,.T.);
#3899=EDGE_CURVE('',#3126,#3125,#1823,.T.);
#3900=EDGE_CURVE('',#3127,#3127,#2633,.T.);
#3901=EDGE_CURVE('',#3128,#3128,#2634,.F.);
#3902=EDGE_CURVE('',#3128,#3127,#1824,.T.);
#3903=EDGE_CURVE('',#3129,#3129,#2635,.F.);
#3904=EDGE_CURVE('',#3129,#3128,#1825,.T.);
#3905=EDGE_CURVE('',#3130,#3130,#2636,.T.);
#3906=EDGE_CURVE('',#3130,#3129,#1826,.T.);
#3907=EDGE_CURVE('',#3131,#3132,#1827,.T.);
#3908=EDGE_CURVE('',#3132,#3133,#1828,.T.);
#3909=EDGE_CURVE('',#3133,#3134,#1829,.T.);
#3910=EDGE_CURVE('',#3131,#3134,#1830,.T.);
#3911=EDGE_CURVE('',#3132,#3135,#1831,.T.);
#3912=EDGE_CURVE('',#3135,#3136,#1832,.T.);
#3913=EDGE_CURVE('',#3136,#3133,#1833,.T.);
#3914=EDGE_CURVE('',#3135,#3137,#1834,.T.);
#3915=EDGE_CURVE('',#3137,#3138,#1835,.T.);
#3916=EDGE_CURVE('',#3138,#3136,#1836,.T.);
#3917=EDGE_CURVE('',#3137,#3139,#1837,.T.);
#3918=EDGE_CURVE('',#3139,#3140,#1838,.T.);
#3919=EDGE_CURVE('',#3140,#3138,#1839,.T.);
#3920=EDGE_CURVE('',#3139,#3141,#1840,.T.);
#3921=EDGE_CURVE('',#3141,#3142,#1841,.T.);
#3922=EDGE_CURVE('',#3142,#3140,#1842,.T.);
#3923=EDGE_CURVE('',#3141,#3131,#1843,.T.);
#3924=EDGE_CURVE('',#3134,#3142,#1844,.T.);
#3925=EDGE_CURVE('',#3143,#3144,#1845,.T.);
#3926=EDGE_CURVE('',#3143,#3145,#1846,.T.);
#3927=EDGE_CURVE('',#3145,#3146,#1847,.T.);
#3928=EDGE_CURVE('',#3144,#3146,#1848,.T.);
#3929=EDGE_CURVE('',#3147,#3143,#1849,.T.);
#3930=EDGE_CURVE('',#3147,#3148,#1850,.T.);
#3931=EDGE_CURVE('',#3148,#3145,#1851,.T.);
#3932=EDGE_CURVE('',#3149,#3147,#1852,.T.);
#3933=EDGE_CURVE('',#3149,#3150,#1853,.T.);
#3934=EDGE_CURVE('',#3150,#3148,#1854,.T.);
#3935=EDGE_CURVE('',#3151,#3149,#1855,.T.);
#3936=EDGE_CURVE('',#3151,#3152,#1856,.T.);
#3937=EDGE_CURVE('',#3152,#3150,#1857,.T.);
#3938=EDGE_CURVE('',#3153,#3151,#1858,.T.);
#3939=EDGE_CURVE('',#3153,#3154,#1859,.T.);
#3940=EDGE_CURVE('',#3154,#3152,#1860,.T.);
#3941=EDGE_CURVE('',#3144,#3153,#1861,.T.);
#3942=EDGE_CURVE('',#3146,#3154,#1862,.T.);
#3943=EDGE_CURVE('',#3155,#3155,#2637,.T.);
#3944=EDGE_CURVE('',#3156,#3156,#2638,.T.);
#3945=EDGE_CURVE('',#3156,#3155,#1863,.T.);
#3946=EDGE_CURVE('',#3157,#3157,#2639,.F.);
#3947=EDGE_CURVE('',#3157,#3156,#1864,.T.);
#3948=EDGE_CURVE('',#3158,#3158,#2640,.T.);
#3949=EDGE_CURVE('',#3158,#3157,#1865,.T.);
#3950=EDGE_CURVE('',#3159,#3160,#1866,.T.);
#3951=EDGE_CURVE('',#3161,#3159,#1867,.T.);
#3952=EDGE_CURVE('',#3162,#3161,#1868,.T.);
#3953=EDGE_CURVE('',#3163,#3162,#1869,.T.);
#3954=EDGE_CURVE('',#3164,#3163,#1870,.T.);
#3955=EDGE_CURVE('',#3165,#3164,#1871,.T.);
#3956=EDGE_CURVE('',#3166,#3165,#1872,.T.);
#3957=EDGE_CURVE('',#3160,#3166,#1873,.T.);
#3958=EDGE_CURVE('',#3163,#3167,#1874,.T.);
#3959=EDGE_CURVE('',#3167,#3168,#1875,.T.);
#3960=EDGE_CURVE('',#3168,#3164,#1876,.T.);
#3961=EDGE_CURVE('',#3169,#3162,#1877,.T.);
#3962=EDGE_CURVE('',#3169,#3167,#1878,.T.);
#3963=EDGE_CURVE('',#3161,#3170,#1879,.T.);
#3964=EDGE_CURVE('',#3170,#3169,#1880,.T.);
#3965=EDGE_CURVE('',#3171,#3159,#1881,.T.);
#3966=EDGE_CURVE('',#3171,#3170,#1882,.T.);
#3967=EDGE_CURVE('',#3172,#3173,#1883,.T.);
#3968=EDGE_CURVE('',#3168,#3172,#1884,.T.);
#3969=EDGE_CURVE('',#3174,#3171,#1885,.T.);
#3970=EDGE_CURVE('',#3173,#3174,#1886,.T.);
#3971=EDGE_CURVE('',#3165,#3172,#1887,.T.);
#3972=EDGE_CURVE('',#3160,#3174,#1888,.T.);
#3973=EDGE_CURVE('',#3173,#3166,#1889,.T.);
#3974=EDGE_CURVE('',#3175,#3175,#2641,.T.);
#3975=EDGE_CURVE('',#3175,#3176,#1890,.T.);
#3976=EDGE_CURVE('',#3176,#3176,#2642,.T.);
#3977=EDGE_CURVE('',#3177,#3177,#2643,.T.);
#3978=EDGE_CURVE('',#3177,#3178,#1891,.T.);
#3979=EDGE_CURVE('',#3178,#3178,#2644,.T.);
#3980=EDGE_CURVE('',#3179,#3180,#11,.T.);
#3981=EDGE_CURVE('',#3181,#3179,#12,.T.);
#3982=EDGE_CURVE('',#3181,#3182,#1892,.T.);
#3983=EDGE_CURVE('',#3182,#3182,#2645,.T.);
#3984=EDGE_CURVE('',#3183,#3181,#13,.T.);
#3985=EDGE_CURVE('',#3184,#3183,#14,.T.);
#3986=EDGE_CURVE('',#3185,#3184,#15,.T.);
#3987=EDGE_CURVE('',#3180,#3185,#16,.T.);
#3988=EDGE_CURVE('',#3186,#3186,#2646,.T.);
#3989=EDGE_CURVE('',#3186,#3187,#1893,.T.);
#3990=EDGE_CURVE('',#3188,#3187,#17,.T.);
#3991=EDGE_CURVE('',#3189,#3188,#18,.T.);
#3992=EDGE_CURVE('',#3190,#3189,#19,.T.);
#3993=EDGE_CURVE('',#3191,#3190,#20,.T.);
#3994=EDGE_CURVE('',#3192,#3191,#21,.T.);
#3995=EDGE_CURVE('',#3187,#3192,#22,.T.);
#3996=EDGE_CURVE('',#3183,#3192,#1894,.T.);
#3997=EDGE_CURVE('',#3184,#3191,#1895,.T.);
#3998=EDGE_CURVE('',#3181,#3187,#1896,.T.);
#3999=EDGE_CURVE('',#3179,#3188,#1897,.T.);
#4000=EDGE_CURVE('',#3193,#3193,#2647,.F.);
#4001=EDGE_CURVE('',#3193,#3194,#1898,.T.);
#4002=EDGE_CURVE('',#3194,#3194,#2648,.F.);
#4003=EDGE_CURVE('',#3180,#3189,#1899,.T.);
#4004=EDGE_CURVE('',#3185,#3190,#1900,.T.);
#4005=ORIENTED_EDGE('',*,*,#3195,.F.);
#4006=ORIENTED_EDGE('',*,*,#3196,.T.);
#4007=ORIENTED_EDGE('',*,*,#3197,.F.);
#4008=ORIENTED_EDGE('',*,*,#3196,.F.);
#4009=ORIENTED_EDGE('',*,*,#3198,.F.);
#4010=ORIENTED_EDGE('',*,*,#3199,.T.);
#4011=ORIENTED_EDGE('',*,*,#3200,.F.);
#4012=ORIENTED_EDGE('',*,*,#3199,.F.);
#4013=ORIENTED_EDGE('',*,*,#3201,.T.);
#4014=ORIENTED_EDGE('',*,*,#3202,.T.);
#4015=ORIENTED_EDGE('',*,*,#3203,.F.);
#4016=ORIENTED_EDGE('',*,*,#3204,.F.);
#4017=ORIENTED_EDGE('',*,*,#3205,.T.);
#4018=ORIENTED_EDGE('',*,*,#3204,.T.);
#4019=ORIENTED_EDGE('',*,*,#3206,.F.);
#4020=ORIENTED_EDGE('',*,*,#3207,.F.);
#4021=ORIENTED_EDGE('',*,*,#3208,.T.);
#4022=ORIENTED_EDGE('',*,*,#3207,.T.);
#4023=ORIENTED_EDGE('',*,*,#3209,.F.);
#4024=ORIENTED_EDGE('',*,*,#3210,.F.);
#4025=ORIENTED_EDGE('',*,*,#3211,.T.);
#4026=ORIENTED_EDGE('',*,*,#3210,.T.);
#4027=ORIENTED_EDGE('',*,*,#3212,.F.);
#4028=ORIENTED_EDGE('',*,*,#3202,.F.);
#4029=ORIENTED_EDGE('',*,*,#3212,.T.);
#4030=ORIENTED_EDGE('',*,*,#3209,.T.);
#4031=ORIENTED_EDGE('',*,*,#3206,.T.);
#4032=ORIENTED_EDGE('',*,*,#3203,.T.);
#4033=ORIENTED_EDGE('',*,*,#3197,.T.);
#4034=ORIENTED_EDGE('',*,*,#3200,.T.);
#4035=ORIENTED_EDGE('',*,*,#3211,.F.);
#4036=ORIENTED_EDGE('',*,*,#3201,.F.);
#4037=ORIENTED_EDGE('',*,*,#3205,.F.);
#4038=ORIENTED_EDGE('',*,*,#3208,.F.);
#4039=ORIENTED_EDGE('',*,*,#3195,.T.);
#4040=ORIENTED_EDGE('',*,*,#3198,.T.);
#4041=ORIENTED_EDGE('',*,*,#3213,.F.);
#4042=ORIENTED_EDGE('',*,*,#3214,.T.);
#4043=ORIENTED_EDGE('',*,*,#3215,.F.);
#4044=ORIENTED_EDGE('',*,*,#3214,.F.);
#4045=ORIENTED_EDGE('',*,*,#3216,.F.);
#4046=ORIENTED_EDGE('',*,*,#3217,.T.);
#4047=ORIENTED_EDGE('',*,*,#3218,.F.);
#4048=ORIENTED_EDGE('',*,*,#3217,.F.);
#4049=ORIENTED_EDGE('',*,*,#3219,.F.);
#4050=ORIENTED_EDGE('',*,*,#3220,.T.);
#4051=ORIENTED_EDGE('',*,*,#3221,.F.);
#4052=ORIENTED_EDGE('',*,*,#3220,.F.);
#4053=ORIENTED_EDGE('',*,*,#3222,.F.);
#4054=ORIENTED_EDGE('',*,*,#3223,.T.);
#4055=ORIENTED_EDGE('',*,*,#3224,.F.);
#4056=ORIENTED_EDGE('',*,*,#3223,.F.);
#4057=ORIENTED_EDGE('',*,*,#3225,.F.);
#4058=ORIENTED_EDGE('',*,*,#3226,.T.);
#4059=ORIENTED_EDGE('',*,*,#3227,.F.);
#4060=ORIENTED_EDGE('',*,*,#3226,.F.);
#4061=ORIENTED_EDGE('',*,*,#3228,.F.);
#4062=ORIENTED_EDGE('',*,*,#3229,.T.);
#4063=ORIENTED_EDGE('',*,*,#3230,.F.);
#4064=ORIENTED_EDGE('',*,*,#3229,.F.);
#4065=ORIENTED_EDGE('',*,*,#3231,.F.);
#4066=ORIENTED_EDGE('',*,*,#3232,.T.);
#4067=ORIENTED_EDGE('',*,*,#3233,.F.);
#4068=ORIENTED_EDGE('',*,*,#3232,.F.);
#4069=ORIENTED_EDGE('',*,*,#3234,.F.);
#4070=ORIENTED_EDGE('',*,*,#3235,.F.);
#4071=ORIENTED_EDGE('',*,*,#3236,.F.);
#4072=ORIENTED_EDGE('',*,*,#3237,.T.);
#4073=ORIENTED_EDGE('',*,*,#3215,.T.);
#4074=ORIENTED_EDGE('',*,*,#3218,.T.);
#4075=ORIENTED_EDGE('',*,*,#3236,.T.);
#4076=ORIENTED_EDGE('',*,*,#3238,.T.);
#4077=ORIENTED_EDGE('',*,*,#3239,.T.);
#4078=ORIENTED_EDGE('',*,*,#3240,.T.);
#4079=ORIENTED_EDGE('',*,*,#3241,.T.);
#4080=ORIENTED_EDGE('',*,*,#3242,.F.);
#4081=ORIENTED_EDGE('',*,*,#3243,.F.);
#4082=ORIENTED_EDGE('',*,*,#3244,.T.);
#4083=ORIENTED_EDGE('',*,*,#3233,.T.);
#4084=ORIENTED_EDGE('',*,*,#3230,.T.);
#4085=ORIENTED_EDGE('',*,*,#3227,.T.);
#4086=ORIENTED_EDGE('',*,*,#3224,.T.);
#4087=ORIENTED_EDGE('',*,*,#3221,.T.);
#4088=ORIENTED_EDGE('',*,*,#3245,.T.);
#4089=ORIENTED_EDGE('',*,*,#3246,.F.);
#4090=ORIENTED_EDGE('',*,*,#3241,.F.);
#4091=ORIENTED_EDGE('',*,*,#3247,.T.);
#4092=ORIENTED_EDGE('',*,*,#3238,.F.);
#4093=ORIENTED_EDGE('',*,*,#3235,.T.);
#4094=ORIENTED_EDGE('',*,*,#3243,.T.);
#4095=ORIENTED_EDGE('',*,*,#3248,.F.);
#4096=ORIENTED_EDGE('',*,*,#3249,.F.);
#4097=ORIENTED_EDGE('',*,*,#3237,.F.);
#4098=ORIENTED_EDGE('',*,*,#3240,.F.);
#4099=ORIENTED_EDGE('',*,*,#3250,.T.);
#4100=ORIENTED_EDGE('',*,*,#3234,.T.);
#4101=ORIENTED_EDGE('',*,*,#3249,.T.);
#4102=ORIENTED_EDGE('',*,*,#3251,.F.);
#4103=ORIENTED_EDGE('',*,*,#3245,.F.);
#4104=ORIENTED_EDGE('',*,*,#3231,.T.);
#4105=ORIENTED_EDGE('',*,*,#3228,.T.);
#4106=ORIENTED_EDGE('',*,*,#3225,.T.);
#4107=ORIENTED_EDGE('',*,*,#3222,.T.);
#4108=ORIENTED_EDGE('',*,*,#3219,.T.);
#4109=ORIENTED_EDGE('',*,*,#3246,.T.);
#4110=ORIENTED_EDGE('',*,*,#3251,.T.);
#4111=ORIENTED_EDGE('',*,*,#3248,.T.);
#4112=ORIENTED_EDGE('',*,*,#3242,.T.);
#4113=ORIENTED_EDGE('',*,*,#3247,.F.);
#4114=ORIENTED_EDGE('',*,*,#3244,.F.);
#4115=ORIENTED_EDGE('',*,*,#3250,.F.);
#4116=ORIENTED_EDGE('',*,*,#3239,.F.);
#4117=ORIENTED_EDGE('',*,*,#3213,.T.);
#4118=ORIENTED_EDGE('',*,*,#3216,.T.);
#4119=ORIENTED_EDGE('',*,*,#3252,.F.);
#4120=ORIENTED_EDGE('',*,*,#3253,.T.);
#4121=ORIENTED_EDGE('',*,*,#3254,.T.);
#4122=ORIENTED_EDGE('',*,*,#3253,.F.);
#4123=ORIENTED_EDGE('',*,*,#3255,.F.);
#4124=ORIENTED_EDGE('',*,*,#3256,.T.);
#4125=ORIENTED_EDGE('',*,*,#3257,.T.);
#4126=ORIENTED_EDGE('',*,*,#3256,.F.);
#4127=ORIENTED_EDGE('',*,*,#3255,.T.);
#4128=ORIENTED_EDGE('',*,*,#3252,.T.);
#4129=ORIENTED_EDGE('',*,*,#3257,.F.);
#4130=ORIENTED_EDGE('',*,*,#3254,.F.);
#4131=ORIENTED_EDGE('',*,*,#3258,.F.);
#4132=ORIENTED_EDGE('',*,*,#3259,.T.);
#4133=ORIENTED_EDGE('',*,*,#3260,.T.);
#4134=ORIENTED_EDGE('',*,*,#3259,.F.);
#4135=ORIENTED_EDGE('',*,*,#3261,.F.);
#4136=ORIENTED_EDGE('',*,*,#3262,.T.);
#4137=ORIENTED_EDGE('',*,*,#3263,.T.);
#4138=ORIENTED_EDGE('',*,*,#3262,.F.);
#4139=ORIENTED_EDGE('',*,*,#3261,.T.);
#4140=ORIENTED_EDGE('',*,*,#3258,.T.);
#4141=ORIENTED_EDGE('',*,*,#3263,.F.);
#4142=ORIENTED_EDGE('',*,*,#3260,.F.);
#4143=ORIENTED_EDGE('',*,*,#3264,.F.);
#4144=ORIENTED_EDGE('',*,*,#3265,.T.);
#4145=ORIENTED_EDGE('',*,*,#3266,.T.);
#4146=ORIENTED_EDGE('',*,*,#3265,.F.);
#4147=ORIENTED_EDGE('',*,*,#3267,.F.);
#4148=ORIENTED_EDGE('',*,*,#3268,.T.);
#4149=ORIENTED_EDGE('',*,*,#3269,.T.);
#4150=ORIENTED_EDGE('',*,*,#3268,.F.);
#4151=ORIENTED_EDGE('',*,*,#3267,.T.);
#4152=ORIENTED_EDGE('',*,*,#3264,.T.);
#4153=ORIENTED_EDGE('',*,*,#3269,.F.);
#4154=ORIENTED_EDGE('',*,*,#3266,.F.);
#4155=ORIENTED_EDGE('',*,*,#3270,.F.);
#4156=ORIENTED_EDGE('',*,*,#3271,.T.);
#4157=ORIENTED_EDGE('',*,*,#3272,.T.);
#4158=ORIENTED_EDGE('',*,*,#3271,.F.);
#4159=ORIENTED_EDGE('',*,*,#3273,.F.);
#4160=ORIENTED_EDGE('',*,*,#3274,.T.);
#4161=ORIENTED_EDGE('',*,*,#3275,.T.);
#4162=ORIENTED_EDGE('',*,*,#3274,.F.);
#4163=ORIENTED_EDGE('',*,*,#3273,.T.);
#4164=ORIENTED_EDGE('',*,*,#3270,.T.);
#4165=ORIENTED_EDGE('',*,*,#3275,.F.);
#4166=ORIENTED_EDGE('',*,*,#3272,.F.);
#4167=ORIENTED_EDGE('',*,*,#3276,.T.);
#4168=ORIENTED_EDGE('',*,*,#3277,.T.);
#4169=ORIENTED_EDGE('',*,*,#3278,.F.);
#4170=ORIENTED_EDGE('',*,*,#3279,.F.);
#4171=ORIENTED_EDGE('',*,*,#3280,.T.);
#4172=ORIENTED_EDGE('',*,*,#3279,.T.);
#4173=ORIENTED_EDGE('',*,*,#3281,.F.);
#4174=ORIENTED_EDGE('',*,*,#3282,.F.);
#4175=ORIENTED_EDGE('',*,*,#3283,.T.);
#4176=ORIENTED_EDGE('',*,*,#3282,.T.);
#4177=ORIENTED_EDGE('',*,*,#3284,.F.);
#4178=ORIENTED_EDGE('',*,*,#3285,.F.);
#4179=ORIENTED_EDGE('',*,*,#3286,.T.);
#4180=ORIENTED_EDGE('',*,*,#3285,.T.);
#4181=ORIENTED_EDGE('',*,*,#3287,.F.);
#4182=ORIENTED_EDGE('',*,*,#3277,.F.);
#4183=ORIENTED_EDGE('',*,*,#3287,.T.);
#4184=ORIENTED_EDGE('',*,*,#3284,.T.);
#4185=ORIENTED_EDGE('',*,*,#3281,.T.);
#4186=ORIENTED_EDGE('',*,*,#3278,.T.);
#4187=ORIENTED_EDGE('',*,*,#3286,.F.);
#4188=ORIENTED_EDGE('',*,*,#3276,.F.);
#4189=ORIENTED_EDGE('',*,*,#3280,.F.);
#4190=ORIENTED_EDGE('',*,*,#3283,.F.);
#4191=ORIENTED_EDGE('',*,*,#3288,.T.);
#4192=ORIENTED_EDGE('',*,*,#3289,.T.);
#4193=ORIENTED_EDGE('',*,*,#3290,.F.);
#4194=ORIENTED_EDGE('',*,*,#3291,.F.);
#4195=ORIENTED_EDGE('',*,*,#3292,.T.);
#4196=ORIENTED_EDGE('',*,*,#3291,.T.);
#4197=ORIENTED_EDGE('',*,*,#3293,.F.);
#4198=ORIENTED_EDGE('',*,*,#3294,.F.);
#4199=ORIENTED_EDGE('',*,*,#3295,.T.);
#4200=ORIENTED_EDGE('',*,*,#3294,.T.);
#4201=ORIENTED_EDGE('',*,*,#3296,.F.);
#4202=ORIENTED_EDGE('',*,*,#3297,.F.);
#4203=ORIENTED_EDGE('',*,*,#3298,.T.);
#4204=ORIENTED_EDGE('',*,*,#3297,.T.);
#4205=ORIENTED_EDGE('',*,*,#3299,.F.);
#4206=ORIENTED_EDGE('',*,*,#3289,.F.);
#4207=ORIENTED_EDGE('',*,*,#3299,.T.);
#4208=ORIENTED_EDGE('',*,*,#3296,.T.);
#4209=ORIENTED_EDGE('',*,*,#3293,.T.);
#4210=ORIENTED_EDGE('',*,*,#3290,.T.);
#4211=ORIENTED_EDGE('',*,*,#3298,.F.);
#4212=ORIENTED_EDGE('',*,*,#3288,.F.);
#4213=ORIENTED_EDGE('',*,*,#3292,.F.);
#4214=ORIENTED_EDGE('',*,*,#3295,.F.);
#4215=ORIENTED_EDGE('',*,*,#3300,.T.);
#4216=ORIENTED_EDGE('',*,*,#3301,.T.);
#4217=ORIENTED_EDGE('',*,*,#3302,.T.);
#4218=ORIENTED_EDGE('',*,*,#3303,.F.);
#4219=ORIENTED_EDGE('',*,*,#3304,.T.);
#4220=ORIENTED_EDGE('',*,*,#3305,.T.);
#4221=ORIENTED_EDGE('',*,*,#3306,.T.);
#4222=ORIENTED_EDGE('',*,*,#3301,.F.);
#4223=ORIENTED_EDGE('',*,*,#3307,.T.);
#4224=ORIENTED_EDGE('',*,*,#3308,.T.);
#4225=ORIENTED_EDGE('',*,*,#3309,.T.);
#4226=ORIENTED_EDGE('',*,*,#3305,.F.);
#4227=ORIENTED_EDGE('',*,*,#3310,.T.);
#4228=ORIENTED_EDGE('',*,*,#3311,.T.);
#4229=ORIENTED_EDGE('',*,*,#3312,.T.);
#4230=ORIENTED_EDGE('',*,*,#3308,.F.);
#4231=ORIENTED_EDGE('',*,*,#3313,.T.);
#4232=ORIENTED_EDGE('',*,*,#3314,.T.);
#4233=ORIENTED_EDGE('',*,*,#3315,.T.);
#4234=ORIENTED_EDGE('',*,*,#3311,.F.);
#4235=ORIENTED_EDGE('',*,*,#3316,.T.);
#4236=ORIENTED_EDGE('',*,*,#3303,.T.);
#4237=ORIENTED_EDGE('',*,*,#3317,.T.);
#4238=ORIENTED_EDGE('',*,*,#3314,.F.);
#4239=ORIENTED_EDGE('',*,*,#3316,.F.);
#4240=ORIENTED_EDGE('',*,*,#3313,.F.);
#4241=ORIENTED_EDGE('',*,*,#3310,.F.);
#4242=ORIENTED_EDGE('',*,*,#3307,.F.);
#4243=ORIENTED_EDGE('',*,*,#3304,.F.);
#4244=ORIENTED_EDGE('',*,*,#3300,.F.);
#4245=ORIENTED_EDGE('',*,*,#3317,.F.);
#4246=ORIENTED_EDGE('',*,*,#3302,.F.);
#4247=ORIENTED_EDGE('',*,*,#3306,.F.);
#4248=ORIENTED_EDGE('',*,*,#3309,.F.);
#4249=ORIENTED_EDGE('',*,*,#3312,.F.);
#4250=ORIENTED_EDGE('',*,*,#3315,.F.);
#4251=ORIENTED_EDGE('',*,*,#3318,.F.);
#4252=ORIENTED_EDGE('',*,*,#3319,.F.);
#4253=ORIENTED_EDGE('',*,*,#3320,.F.);
#4254=ORIENTED_EDGE('',*,*,#3321,.T.);
#4255=ORIENTED_EDGE('',*,*,#3319,.T.);
#4256=ORIENTED_EDGE('',*,*,#3321,.F.);
#4257=ORIENTED_EDGE('',*,*,#3322,.F.);
#4258=ORIENTED_EDGE('',*,*,#3323,.T.);
#4259=ORIENTED_EDGE('',*,*,#3320,.T.);
#4260=ORIENTED_EDGE('',*,*,#3323,.F.);
#4261=ORIENTED_EDGE('',*,*,#3324,.F.);
#4262=ORIENTED_EDGE('',*,*,#3325,.T.);
#4263=ORIENTED_EDGE('',*,*,#3322,.T.);
#4264=ORIENTED_EDGE('',*,*,#3325,.F.);
#4265=ORIENTED_EDGE('',*,*,#3324,.T.);
#4266=ORIENTED_EDGE('',*,*,#3326,.F.);
#4267=ORIENTED_EDGE('',*,*,#3327,.F.);
#4268=ORIENTED_EDGE('',*,*,#3328,.T.);
#4269=ORIENTED_EDGE('',*,*,#3326,.T.);
#4270=ORIENTED_EDGE('',*,*,#3328,.F.);
#4271=ORIENTED_EDGE('',*,*,#3318,.T.);
#4272=ORIENTED_EDGE('',*,*,#3329,.T.);
#4273=ORIENTED_EDGE('',*,*,#3327,.T.);
#4274=ORIENTED_EDGE('',*,*,#3329,.F.);
#4275=ORIENTED_EDGE('',*,*,#3330,.F.);
#4276=ORIENTED_EDGE('',*,*,#3331,.T.);
#4277=ORIENTED_EDGE('',*,*,#3332,.F.);
#4278=ORIENTED_EDGE('',*,*,#3331,.F.);
#4279=ORIENTED_EDGE('',*,*,#3333,.F.);
#4280=ORIENTED_EDGE('',*,*,#3334,.T.);
#4281=ORIENTED_EDGE('',*,*,#3335,.F.);
#4282=ORIENTED_EDGE('',*,*,#3334,.F.);
#4283=ORIENTED_EDGE('',*,*,#3336,.T.);
#4284=ORIENTED_EDGE('',*,*,#3336,.F.);
#4285=ORIENTED_EDGE('',*,*,#3333,.T.);
#4286=ORIENTED_EDGE('',*,*,#3332,.T.);
#4287=ORIENTED_EDGE('',*,*,#3337,.F.);
#4288=ORIENTED_EDGE('',*,*,#3338,.T.);
#4289=ORIENTED_EDGE('',*,*,#3339,.F.);
#4290=ORIENTED_EDGE('',*,*,#3338,.F.);
#4291=ORIENTED_EDGE('',*,*,#3340,.F.);
#4292=ORIENTED_EDGE('',*,*,#3341,.T.);
#4293=ORIENTED_EDGE('',*,*,#3342,.F.);
#4294=ORIENTED_EDGE('',*,*,#3341,.F.);
#4295=ORIENTED_EDGE('',*,*,#3339,.T.);
#4296=ORIENTED_EDGE('',*,*,#3330,.T.);
#4297=ORIENTED_EDGE('',*,*,#3340,.T.);
#4298=ORIENTED_EDGE('',*,*,#3335,.T.);
#4299=ORIENTED_EDGE('',*,*,#3343,.F.);
#4300=ORIENTED_EDGE('',*,*,#3344,.T.);
#4301=ORIENTED_EDGE('',*,*,#3345,.F.);
#4302=ORIENTED_EDGE('',*,*,#3344,.F.);
#4303=ORIENTED_EDGE('',*,*,#3346,.F.);
#4304=ORIENTED_EDGE('',*,*,#3347,.T.);
#4305=ORIENTED_EDGE('',*,*,#3348,.F.);
#4306=ORIENTED_EDGE('',*,*,#3347,.F.);
#4307=ORIENTED_EDGE('',*,*,#3349,.F.);
#4308=ORIENTED_EDGE('',*,*,#3350,.T.);
#4309=ORIENTED_EDGE('',*,*,#3351,.F.);
#4310=ORIENTED_EDGE('',*,*,#3350,.F.);
#4311=ORIENTED_EDGE('',*,*,#3352,.F.);
#4312=ORIENTED_EDGE('',*,*,#3353,.T.);
#4313=ORIENTED_EDGE('',*,*,#3354,.F.);
#4314=ORIENTED_EDGE('',*,*,#3353,.F.);
#4315=ORIENTED_EDGE('',*,*,#3355,.T.);
#4316=ORIENTED_EDGE('',*,*,#3356,.T.);
#4317=ORIENTED_EDGE('',*,*,#3357,.F.);
#4318=ORIENTED_EDGE('',*,*,#3358,.F.);
#4319=ORIENTED_EDGE('',*,*,#3359,.T.);
#4320=ORIENTED_EDGE('',*,*,#3358,.T.);
#4321=ORIENTED_EDGE('',*,*,#3360,.F.);
#4322=ORIENTED_EDGE('',*,*,#3361,.F.);
#4323=ORIENTED_EDGE('',*,*,#3362,.T.);
#4324=ORIENTED_EDGE('',*,*,#3361,.T.);
#4325=ORIENTED_EDGE('',*,*,#3363,.F.);
#4326=ORIENTED_EDGE('',*,*,#3364,.F.);
#4327=ORIENTED_EDGE('',*,*,#3365,.T.);
#4328=ORIENTED_EDGE('',*,*,#3364,.T.);
#4329=ORIENTED_EDGE('',*,*,#3366,.F.);
#4330=ORIENTED_EDGE('',*,*,#3367,.F.);
#4331=ORIENTED_EDGE('',*,*,#3368,.T.);
#4332=ORIENTED_EDGE('',*,*,#3367,.T.);
#4333=ORIENTED_EDGE('',*,*,#3369,.F.);
#4334=ORIENTED_EDGE('',*,*,#3370,.F.);
#4335=ORIENTED_EDGE('',*,*,#3371,.T.);
#4336=ORIENTED_EDGE('',*,*,#3370,.T.);
#4337=ORIENTED_EDGE('',*,*,#3372,.F.);
#4338=ORIENTED_EDGE('',*,*,#3373,.F.);
#4339=ORIENTED_EDGE('',*,*,#3374,.T.);
#4340=ORIENTED_EDGE('',*,*,#3373,.T.);
#4341=ORIENTED_EDGE('',*,*,#3375,.F.);
#4342=ORIENTED_EDGE('',*,*,#3376,.F.);
#4343=ORIENTED_EDGE('',*,*,#3377,.T.);
#4344=ORIENTED_EDGE('',*,*,#3376,.T.);
#4345=ORIENTED_EDGE('',*,*,#3378,.F.);
#4346=ORIENTED_EDGE('',*,*,#3356,.F.);
#4347=ORIENTED_EDGE('',*,*,#3378,.T.);
#4348=ORIENTED_EDGE('',*,*,#3375,.T.);
#4349=ORIENTED_EDGE('',*,*,#3372,.T.);
#4350=ORIENTED_EDGE('',*,*,#3369,.T.);
#4351=ORIENTED_EDGE('',*,*,#3366,.T.);
#4352=ORIENTED_EDGE('',*,*,#3363,.T.);
#4353=ORIENTED_EDGE('',*,*,#3360,.T.);
#4354=ORIENTED_EDGE('',*,*,#3357,.T.);
#4355=ORIENTED_EDGE('',*,*,#3342,.T.);
#4356=ORIENTED_EDGE('',*,*,#3345,.T.);
#4357=ORIENTED_EDGE('',*,*,#3348,.T.);
#4358=ORIENTED_EDGE('',*,*,#3351,.T.);
#4359=ORIENTED_EDGE('',*,*,#3354,.T.);
#4360=ORIENTED_EDGE('',*,*,#3377,.F.);
#4361=ORIENTED_EDGE('',*,*,#3355,.F.);
#4362=ORIENTED_EDGE('',*,*,#3359,.F.);
#4363=ORIENTED_EDGE('',*,*,#3362,.F.);
#4364=ORIENTED_EDGE('',*,*,#3365,.F.);
#4365=ORIENTED_EDGE('',*,*,#3368,.F.);
#4366=ORIENTED_EDGE('',*,*,#3371,.F.);
#4367=ORIENTED_EDGE('',*,*,#3374,.F.);
#4368=ORIENTED_EDGE('',*,*,#3337,.T.);
#4369=ORIENTED_EDGE('',*,*,#3343,.T.);
#4370=ORIENTED_EDGE('',*,*,#3346,.T.);
#4371=ORIENTED_EDGE('',*,*,#3349,.T.);
#4372=ORIENTED_EDGE('',*,*,#3352,.T.);
#4373=ORIENTED_EDGE('',*,*,#3379,.T.);
#4374=ORIENTED_EDGE('',*,*,#3380,.T.);
#4375=ORIENTED_EDGE('',*,*,#3381,.F.);
#4376=ORIENTED_EDGE('',*,*,#3380,.F.);
#4377=ORIENTED_EDGE('',*,*,#3382,.F.);
#4378=ORIENTED_EDGE('',*,*,#3381,.T.);
#4379=ORIENTED_EDGE('',*,*,#3383,.T.);
#4380=ORIENTED_EDGE('',*,*,#3383,.F.);
#4381=ORIENTED_EDGE('',*,*,#3382,.T.);
#4382=ORIENTED_EDGE('',*,*,#3384,.F.);
#4383=ORIENTED_EDGE('',*,*,#3384,.T.);
#4384=ORIENTED_EDGE('',*,*,#3379,.F.);
#4385=ORIENTED_EDGE('',*,*,#3385,.F.);
#4386=ORIENTED_EDGE('',*,*,#3386,.F.);
#4387=ORIENTED_EDGE('',*,*,#3387,.F.);
#4388=ORIENTED_EDGE('',*,*,#3388,.T.);
#4389=ORIENTED_EDGE('',*,*,#3389,.F.);
#4390=ORIENTED_EDGE('',*,*,#3388,.F.);
#4391=ORIENTED_EDGE('',*,*,#3390,.F.);
#4392=ORIENTED_EDGE('',*,*,#3391,.T.);
#4393=ORIENTED_EDGE('',*,*,#3392,.F.);
#4394=ORIENTED_EDGE('',*,*,#3393,.F.);
#4395=ORIENTED_EDGE('',*,*,#3394,.F.);
#4396=ORIENTED_EDGE('',*,*,#3391,.F.);
#4397=ORIENTED_EDGE('',*,*,#3395,.F.);
#4398=ORIENTED_EDGE('',*,*,#3396,.T.);
#4399=ORIENTED_EDGE('',*,*,#3397,.T.);
#4400=ORIENTED_EDGE('',*,*,#3396,.F.);
#4401=ORIENTED_EDGE('',*,*,#3386,.T.);
#4402=ORIENTED_EDGE('',*,*,#3385,.T.);
#4403=ORIENTED_EDGE('',*,*,#3387,.T.);
#4404=ORIENTED_EDGE('',*,*,#3393,.T.);
#4405=ORIENTED_EDGE('',*,*,#3392,.T.);
#4406=ORIENTED_EDGE('',*,*,#3394,.T.);
#4407=ORIENTED_EDGE('',*,*,#3398,.T.);
#4408=ORIENTED_EDGE('',*,*,#3399,.T.);
#4409=ORIENTED_EDGE('',*,*,#3400,.T.);
#4410=ORIENTED_EDGE('',*,*,#3401,.T.);
#4411=ORIENTED_EDGE('',*,*,#3402,.T.);
#4412=ORIENTED_EDGE('',*,*,#3403,.T.);
#4413=ORIENTED_EDGE('',*,*,#3404,.T.);
#4414=ORIENTED_EDGE('',*,*,#3405,.T.);
#4415=ORIENTED_EDGE('',*,*,#3406,.T.);
#4416=ORIENTED_EDGE('',*,*,#3407,.T.);
#4417=ORIENTED_EDGE('',*,*,#3408,.T.);
#4418=ORIENTED_EDGE('',*,*,#3409,.T.);
#4419=ORIENTED_EDGE('',*,*,#3399,.F.);
#4420=ORIENTED_EDGE('',*,*,#3398,.F.);
#4421=ORIENTED_EDGE('',*,*,#3400,.F.);
#4422=ORIENTED_EDGE('',*,*,#3410,.T.);
#4423=ORIENTED_EDGE('',*,*,#3411,.F.);
#4424=ORIENTED_EDGE('',*,*,#3410,.F.);
#4425=ORIENTED_EDGE('',*,*,#3412,.F.);
#4426=ORIENTED_EDGE('',*,*,#3413,.T.);
#4427=ORIENTED_EDGE('',*,*,#3402,.F.);
#4428=ORIENTED_EDGE('',*,*,#3401,.F.);
#4429=ORIENTED_EDGE('',*,*,#3403,.F.);
#4430=ORIENTED_EDGE('',*,*,#3413,.F.);
#4431=ORIENTED_EDGE('',*,*,#3405,.F.);
#4432=ORIENTED_EDGE('',*,*,#3404,.F.);
#4433=ORIENTED_EDGE('',*,*,#3406,.F.);
#4434=ORIENTED_EDGE('',*,*,#3414,.T.);
#4435=ORIENTED_EDGE('',*,*,#3415,.F.);
#4436=ORIENTED_EDGE('',*,*,#3414,.F.);
#4437=ORIENTED_EDGE('',*,*,#3416,.F.);
#4438=ORIENTED_EDGE('',*,*,#3417,.T.);
#4439=ORIENTED_EDGE('',*,*,#3408,.F.);
#4440=ORIENTED_EDGE('',*,*,#3407,.F.);
#4441=ORIENTED_EDGE('',*,*,#3409,.F.);
#4442=ORIENTED_EDGE('',*,*,#3417,.F.);
#4443=ORIENTED_EDGE('',*,*,#3397,.F.);
#4444=ORIENTED_EDGE('',*,*,#3418,.T.);
#4445=ORIENTED_EDGE('',*,*,#3419,.F.);
#4446=ORIENTED_EDGE('',*,*,#3395,.T.);
#4447=ORIENTED_EDGE('',*,*,#3420,.F.);
#4448=ORIENTED_EDGE('',*,*,#3421,.T.);
#4449=ORIENTED_EDGE('',*,*,#3419,.T.);
#4450=ORIENTED_EDGE('',*,*,#3421,.F.);
#4451=ORIENTED_EDGE('',*,*,#3420,.T.);
#4452=ORIENTED_EDGE('',*,*,#3422,.F.);
#4453=ORIENTED_EDGE('',*,*,#3422,.T.);
#4454=ORIENTED_EDGE('',*,*,#3423,.T.);
#4455=ORIENTED_EDGE('',*,*,#3418,.F.);
#4456=ORIENTED_EDGE('',*,*,#3423,.F.);
#4457=ORIENTED_EDGE('',*,*,#3390,.T.);
#4458=ORIENTED_EDGE('',*,*,#3389,.T.);
#4459=ORIENTED_EDGE('',*,*,#3412,.T.);
#4460=ORIENTED_EDGE('',*,*,#3411,.T.);
#4461=ORIENTED_EDGE('',*,*,#3416,.T.);
#4462=ORIENTED_EDGE('',*,*,#3415,.T.);
#4463=ORIENTED_EDGE('',*,*,#3424,.F.);
#4464=ORIENTED_EDGE('',*,*,#3425,.F.);
#4465=ORIENTED_EDGE('',*,*,#3426,.T.);
#4466=ORIENTED_EDGE('',*,*,#3424,.T.);
#4467=ORIENTED_EDGE('',*,*,#3426,.F.);
#4468=ORIENTED_EDGE('',*,*,#3427,.F.);
#4469=ORIENTED_EDGE('',*,*,#3428,.T.);
#4470=ORIENTED_EDGE('',*,*,#3425,.T.);
#4471=ORIENTED_EDGE('',*,*,#3428,.F.);
#4472=ORIENTED_EDGE('',*,*,#3429,.F.);
#4473=ORIENTED_EDGE('',*,*,#3430,.T.);
#4474=ORIENTED_EDGE('',*,*,#3427,.T.);
#4475=ORIENTED_EDGE('',*,*,#3430,.F.);
#4476=ORIENTED_EDGE('',*,*,#3429,.T.);
#4477=ORIENTED_EDGE('',*,*,#3431,.F.);
#4478=ORIENTED_EDGE('',*,*,#3432,.F.);
#4479=ORIENTED_EDGE('',*,*,#3433,.T.);
#4480=ORIENTED_EDGE('',*,*,#3431,.T.);
#4481=ORIENTED_EDGE('',*,*,#3433,.F.);
#4482=ORIENTED_EDGE('',*,*,#3434,.F.);
#4483=ORIENTED_EDGE('',*,*,#3435,.T.);
#4484=ORIENTED_EDGE('',*,*,#3432,.T.);
#4485=ORIENTED_EDGE('',*,*,#3435,.F.);
#4486=ORIENTED_EDGE('',*,*,#3436,.F.);
#4487=ORIENTED_EDGE('',*,*,#3437,.T.);
#4488=ORIENTED_EDGE('',*,*,#3434,.T.);
#4489=ORIENTED_EDGE('',*,*,#3437,.F.);
#4490=ORIENTED_EDGE('',*,*,#3436,.T.);
#4491=ORIENTED_EDGE('',*,*,#3438,.T.);
#4492=ORIENTED_EDGE('',*,*,#3439,.T.);
#4493=ORIENTED_EDGE('',*,*,#3440,.T.);
#4494=ORIENTED_EDGE('',*,*,#3441,.F.);
#4495=ORIENTED_EDGE('',*,*,#3442,.T.);
#4496=ORIENTED_EDGE('',*,*,#3443,.T.);
#4497=ORIENTED_EDGE('',*,*,#3444,.T.);
#4498=ORIENTED_EDGE('',*,*,#3439,.F.);
#4499=ORIENTED_EDGE('',*,*,#3445,.T.);
#4500=ORIENTED_EDGE('',*,*,#3446,.T.);
#4501=ORIENTED_EDGE('',*,*,#3447,.T.);
#4502=ORIENTED_EDGE('',*,*,#3443,.F.);
#4503=ORIENTED_EDGE('',*,*,#3448,.T.);
#4504=ORIENTED_EDGE('',*,*,#3449,.T.);
#4505=ORIENTED_EDGE('',*,*,#3450,.T.);
#4506=ORIENTED_EDGE('',*,*,#3446,.F.);
#4507=ORIENTED_EDGE('',*,*,#3451,.T.);
#4508=ORIENTED_EDGE('',*,*,#3452,.T.);
#4509=ORIENTED_EDGE('',*,*,#3453,.T.);
#4510=ORIENTED_EDGE('',*,*,#3449,.F.);
#4511=ORIENTED_EDGE('',*,*,#3454,.T.);
#4512=ORIENTED_EDGE('',*,*,#3441,.T.);
#4513=ORIENTED_EDGE('',*,*,#3455,.T.);
#4514=ORIENTED_EDGE('',*,*,#3452,.F.);
#4515=ORIENTED_EDGE('',*,*,#3454,.F.);
#4516=ORIENTED_EDGE('',*,*,#3451,.F.);
#4517=ORIENTED_EDGE('',*,*,#3448,.F.);
#4518=ORIENTED_EDGE('',*,*,#3445,.F.);
#4519=ORIENTED_EDGE('',*,*,#3442,.F.);
#4520=ORIENTED_EDGE('',*,*,#3438,.F.);
#4521=ORIENTED_EDGE('',*,*,#3455,.F.);
#4522=ORIENTED_EDGE('',*,*,#3440,.F.);
#4523=ORIENTED_EDGE('',*,*,#3444,.F.);
#4524=ORIENTED_EDGE('',*,*,#3447,.F.);
#4525=ORIENTED_EDGE('',*,*,#3450,.F.);
#4526=ORIENTED_EDGE('',*,*,#3453,.F.);
#4527=ORIENTED_EDGE('',*,*,#3456,.F.);
#4528=ORIENTED_EDGE('',*,*,#3457,.T.);
#4529=ORIENTED_EDGE('',*,*,#3458,.F.);
#4530=ORIENTED_EDGE('',*,*,#3459,.T.);
#4531=ORIENTED_EDGE('',*,*,#3460,.F.);
#4532=ORIENTED_EDGE('',*,*,#3459,.F.);
#4533=ORIENTED_EDGE('',*,*,#3461,.F.);
#4534=ORIENTED_EDGE('',*,*,#3462,.F.);
#4535=ORIENTED_EDGE('',*,*,#3463,.F.);
#4536=ORIENTED_EDGE('',*,*,#3462,.T.);
#4537=ORIENTED_EDGE('',*,*,#3464,.T.);
#4538=ORIENTED_EDGE('',*,*,#3465,.T.);
#4539=ORIENTED_EDGE('',*,*,#3461,.T.);
#4540=ORIENTED_EDGE('',*,*,#3458,.T.);
#4541=ORIENTED_EDGE('',*,*,#3466,.T.);
#4542=ORIENTED_EDGE('',*,*,#3464,.F.);
#4543=ORIENTED_EDGE('',*,*,#3467,.F.);
#4544=ORIENTED_EDGE('',*,*,#3465,.F.);
#4545=ORIENTED_EDGE('',*,*,#3466,.F.);
#4546=ORIENTED_EDGE('',*,*,#3457,.F.);
#4547=ORIENTED_EDGE('',*,*,#3468,.F.);
#4548=ORIENTED_EDGE('',*,*,#3469,.T.);
#4549=ORIENTED_EDGE('',*,*,#3470,.T.);
#4550=ORIENTED_EDGE('',*,*,#3469,.F.);
#4551=ORIENTED_EDGE('',*,*,#3470,.F.);
#4552=ORIENTED_EDGE('',*,*,#3471,.F.);
#4553=ORIENTED_EDGE('',*,*,#3472,.T.);
#4554=ORIENTED_EDGE('',*,*,#3473,.F.);
#4555=ORIENTED_EDGE('',*,*,#3474,.T.);
#4556=ORIENTED_EDGE('',*,*,#3475,.F.);
#4557=ORIENTED_EDGE('',*,*,#3474,.F.);
#4558=ORIENTED_EDGE('',*,*,#3476,.F.);
#4559=ORIENTED_EDGE('',*,*,#3477,.F.);
#4560=ORIENTED_EDGE('',*,*,#3478,.F.);
#4561=ORIENTED_EDGE('',*,*,#3477,.T.);
#4562=ORIENTED_EDGE('',*,*,#3479,.T.);
#4563=ORIENTED_EDGE('',*,*,#3480,.T.);
#4564=ORIENTED_EDGE('',*,*,#3476,.T.);
#4565=ORIENTED_EDGE('',*,*,#3473,.T.);
#4566=ORIENTED_EDGE('',*,*,#3481,.T.);
#4567=ORIENTED_EDGE('',*,*,#3479,.F.);
#4568=ORIENTED_EDGE('',*,*,#3482,.F.);
#4569=ORIENTED_EDGE('',*,*,#3480,.F.);
#4570=ORIENTED_EDGE('',*,*,#3481,.F.);
#4571=ORIENTED_EDGE('',*,*,#3472,.F.);
#4572=ORIENTED_EDGE('',*,*,#3483,.F.);
#4573=ORIENTED_EDGE('',*,*,#3484,.T.);
#4574=ORIENTED_EDGE('',*,*,#3485,.F.);
#4575=ORIENTED_EDGE('',*,*,#3484,.F.);
#4576=ORIENTED_EDGE('',*,*,#3483,.T.);
#4577=ORIENTED_EDGE('',*,*,#3486,.F.);
#4578=ORIENTED_EDGE('',*,*,#3487,.T.);
#4579=ORIENTED_EDGE('',*,*,#3488,.T.);
#4580=ORIENTED_EDGE('',*,*,#3487,.F.);
#4581=ORIENTED_EDGE('',*,*,#3478,.T.);
#4582=ORIENTED_EDGE('',*,*,#3482,.T.);
#4583=ORIENTED_EDGE('',*,*,#3471,.T.);
#4584=ORIENTED_EDGE('',*,*,#3475,.T.);
#4585=ORIENTED_EDGE('',*,*,#3488,.F.);
#4586=ORIENTED_EDGE('',*,*,#3468,.T.);
#4587=ORIENTED_EDGE('',*,*,#3489,.F.);
#4588=ORIENTED_EDGE('',*,*,#3490,.T.);
#4589=ORIENTED_EDGE('',*,*,#3491,.T.);
#4590=ORIENTED_EDGE('',*,*,#3490,.F.);
#4591=ORIENTED_EDGE('',*,*,#3463,.T.);
#4592=ORIENTED_EDGE('',*,*,#3467,.T.);
#4593=ORIENTED_EDGE('',*,*,#3456,.T.);
#4594=ORIENTED_EDGE('',*,*,#3460,.T.);
#4595=ORIENTED_EDGE('',*,*,#3489,.T.);
#4596=ORIENTED_EDGE('',*,*,#3485,.T.);
#4597=ORIENTED_EDGE('',*,*,#3491,.F.);
#4598=ORIENTED_EDGE('',*,*,#3486,.T.);
#4599=ORIENTED_EDGE('',*,*,#3492,.F.);
#4600=ORIENTED_EDGE('',*,*,#3493,.T.);
#4601=ORIENTED_EDGE('',*,*,#3494,.T.);
#4602=ORIENTED_EDGE('',*,*,#3493,.F.);
#4603=ORIENTED_EDGE('',*,*,#3495,.F.);
#4604=ORIENTED_EDGE('',*,*,#3496,.T.);
#4605=ORIENTED_EDGE('',*,*,#3497,.T.);
#4606=ORIENTED_EDGE('',*,*,#3496,.F.);
#4607=ORIENTED_EDGE('',*,*,#3495,.T.);
#4608=ORIENTED_EDGE('',*,*,#3492,.T.);
#4609=ORIENTED_EDGE('',*,*,#3497,.F.);
#4610=ORIENTED_EDGE('',*,*,#3494,.F.);
#4611=ORIENTED_EDGE('',*,*,#3498,.F.);
#4612=ORIENTED_EDGE('',*,*,#3499,.T.);
#4613=ORIENTED_EDGE('',*,*,#3500,.T.);
#4614=ORIENTED_EDGE('',*,*,#3499,.F.);
#4615=ORIENTED_EDGE('',*,*,#3501,.F.);
#4616=ORIENTED_EDGE('',*,*,#3502,.T.);
#4617=ORIENTED_EDGE('',*,*,#3503,.T.);
#4618=ORIENTED_EDGE('',*,*,#3502,.F.);
#4619=ORIENTED_EDGE('',*,*,#3501,.T.);
#4620=ORIENTED_EDGE('',*,*,#3498,.T.);
#4621=ORIENTED_EDGE('',*,*,#3503,.F.);
#4622=ORIENTED_EDGE('',*,*,#3500,.F.);
#4623=ORIENTED_EDGE('',*,*,#3504,.F.);
#4624=ORIENTED_EDGE('',*,*,#3505,.T.);
#4625=ORIENTED_EDGE('',*,*,#3506,.T.);
#4626=ORIENTED_EDGE('',*,*,#3505,.F.);
#4627=ORIENTED_EDGE('',*,*,#3507,.F.);
#4628=ORIENTED_EDGE('',*,*,#3508,.T.);
#4629=ORIENTED_EDGE('',*,*,#3509,.T.);
#4630=ORIENTED_EDGE('',*,*,#3508,.F.);
#4631=ORIENTED_EDGE('',*,*,#3507,.T.);
#4632=ORIENTED_EDGE('',*,*,#3504,.T.);
#4633=ORIENTED_EDGE('',*,*,#3509,.F.);
#4634=ORIENTED_EDGE('',*,*,#3506,.F.);
#4635=ORIENTED_EDGE('',*,*,#3510,.F.);
#4636=ORIENTED_EDGE('',*,*,#3511,.T.);
#4637=ORIENTED_EDGE('',*,*,#3512,.F.);
#4638=ORIENTED_EDGE('',*,*,#3513,.F.);
#4639=ORIENTED_EDGE('',*,*,#3514,.T.);
#4640=ORIENTED_EDGE('',*,*,#3515,.F.);
#4641=ORIENTED_EDGE('',*,*,#3516,.F.);
#4642=ORIENTED_EDGE('',*,*,#3514,.F.);
#4643=ORIENTED_EDGE('',*,*,#3517,.F.);
#4644=ORIENTED_EDGE('',*,*,#3518,.F.);
#4645=ORIENTED_EDGE('',*,*,#3511,.F.);
#4646=ORIENTED_EDGE('',*,*,#3519,.F.);
#4647=ORIENTED_EDGE('',*,*,#3517,.T.);
#4648=ORIENTED_EDGE('',*,*,#3513,.T.);
#4649=ORIENTED_EDGE('',*,*,#3520,.F.);
#4650=ORIENTED_EDGE('',*,*,#3521,.T.);
#4651=ORIENTED_EDGE('',*,*,#3522,.T.);
#4652=ORIENTED_EDGE('',*,*,#3521,.F.);
#4653=ORIENTED_EDGE('',*,*,#3518,.T.);
#4654=ORIENTED_EDGE('',*,*,#3519,.T.);
#4655=ORIENTED_EDGE('',*,*,#3512,.T.);
#4656=ORIENTED_EDGE('',*,*,#3510,.T.);
#4657=ORIENTED_EDGE('',*,*,#3523,.F.);
#4658=ORIENTED_EDGE('',*,*,#3524,.T.);
#4659=ORIENTED_EDGE('',*,*,#3525,.T.);
#4660=ORIENTED_EDGE('',*,*,#3524,.F.);
#4661=ORIENTED_EDGE('',*,*,#3515,.T.);
#4662=ORIENTED_EDGE('',*,*,#3516,.T.);
#4663=ORIENTED_EDGE('',*,*,#3523,.T.);
#4664=ORIENTED_EDGE('',*,*,#3520,.T.);
#4665=ORIENTED_EDGE('',*,*,#3525,.F.);
#4666=ORIENTED_EDGE('',*,*,#3522,.F.);
#4667=ORIENTED_EDGE('',*,*,#3526,.F.);
#4668=ORIENTED_EDGE('',*,*,#3527,.T.);
#4669=ORIENTED_EDGE('',*,*,#3528,.F.);
#4670=ORIENTED_EDGE('',*,*,#3529,.F.);
#4671=ORIENTED_EDGE('',*,*,#3530,.T.);
#4672=ORIENTED_EDGE('',*,*,#3531,.F.);
#4673=ORIENTED_EDGE('',*,*,#3532,.F.);
#4674=ORIENTED_EDGE('',*,*,#3530,.F.);
#4675=ORIENTED_EDGE('',*,*,#3533,.F.);
#4676=ORIENTED_EDGE('',*,*,#3534,.F.);
#4677=ORIENTED_EDGE('',*,*,#3527,.F.);
#4678=ORIENTED_EDGE('',*,*,#3535,.F.);
#4679=ORIENTED_EDGE('',*,*,#3533,.T.);
#4680=ORIENTED_EDGE('',*,*,#3529,.T.);
#4681=ORIENTED_EDGE('',*,*,#3536,.F.);
#4682=ORIENTED_EDGE('',*,*,#3537,.T.);
#4683=ORIENTED_EDGE('',*,*,#3538,.T.);
#4684=ORIENTED_EDGE('',*,*,#3537,.F.);
#4685=ORIENTED_EDGE('',*,*,#3534,.T.);
#4686=ORIENTED_EDGE('',*,*,#3535,.T.);
#4687=ORIENTED_EDGE('',*,*,#3528,.T.);
#4688=ORIENTED_EDGE('',*,*,#3526,.T.);
#4689=ORIENTED_EDGE('',*,*,#3539,.F.);
#4690=ORIENTED_EDGE('',*,*,#3540,.T.);
#4691=ORIENTED_EDGE('',*,*,#3541,.T.);
#4692=ORIENTED_EDGE('',*,*,#3540,.F.);
#4693=ORIENTED_EDGE('',*,*,#3531,.T.);
#4694=ORIENTED_EDGE('',*,*,#3532,.T.);
#4695=ORIENTED_EDGE('',*,*,#3539,.T.);
#4696=ORIENTED_EDGE('',*,*,#3536,.T.);
#4697=ORIENTED_EDGE('',*,*,#3541,.F.);
#4698=ORIENTED_EDGE('',*,*,#3538,.F.);
#4699=ORIENTED_EDGE('',*,*,#3542,.F.);
#4700=ORIENTED_EDGE('',*,*,#3543,.T.);
#4701=ORIENTED_EDGE('',*,*,#3544,.F.);
#4702=ORIENTED_EDGE('',*,*,#3545,.F.);
#4703=ORIENTED_EDGE('',*,*,#3546,.F.);
#4704=ORIENTED_EDGE('',*,*,#3547,.T.);
#4705=ORIENTED_EDGE('',*,*,#3548,.F.);
#4706=ORIENTED_EDGE('',*,*,#3543,.F.);
#4707=ORIENTED_EDGE('',*,*,#3549,.F.);
#4708=ORIENTED_EDGE('',*,*,#3550,.F.);
#4709=ORIENTED_EDGE('',*,*,#3551,.F.);
#4710=ORIENTED_EDGE('',*,*,#3547,.F.);
#4711=ORIENTED_EDGE('',*,*,#3552,.T.);
#4712=ORIENTED_EDGE('',*,*,#3553,.T.);
#4713=ORIENTED_EDGE('',*,*,#3554,.T.);
#4714=ORIENTED_EDGE('',*,*,#3555,.T.);
#4715=ORIENTED_EDGE('',*,*,#3556,.T.);
#4716=ORIENTED_EDGE('',*,*,#3557,.T.);
#4717=ORIENTED_EDGE('',*,*,#3558,.T.);
#4718=ORIENTED_EDGE('',*,*,#3544,.T.);
#4719=ORIENTED_EDGE('',*,*,#3548,.T.);
#4720=ORIENTED_EDGE('',*,*,#3551,.T.);
#4721=ORIENTED_EDGE('',*,*,#3559,.T.);
#4722=ORIENTED_EDGE('',*,*,#3545,.T.);
#4723=ORIENTED_EDGE('',*,*,#3559,.F.);
#4724=ORIENTED_EDGE('',*,*,#3550,.T.);
#4725=ORIENTED_EDGE('',*,*,#3560,.T.);
#4726=ORIENTED_EDGE('',*,*,#3561,.F.);
#4727=ORIENTED_EDGE('',*,*,#3562,.T.);
#4728=ORIENTED_EDGE('',*,*,#3553,.F.);
#4729=ORIENTED_EDGE('',*,*,#3562,.F.);
#4730=ORIENTED_EDGE('',*,*,#3563,.F.);
#4731=ORIENTED_EDGE('',*,*,#3564,.T.);
#4732=ORIENTED_EDGE('',*,*,#3554,.F.);
#4733=ORIENTED_EDGE('',*,*,#3564,.F.);
#4734=ORIENTED_EDGE('',*,*,#3565,.F.);
#4735=ORIENTED_EDGE('',*,*,#3566,.T.);
#4736=ORIENTED_EDGE('',*,*,#3555,.F.);
#4737=ORIENTED_EDGE('',*,*,#3566,.F.);
#4738=ORIENTED_EDGE('',*,*,#3567,.F.);
#4739=ORIENTED_EDGE('',*,*,#3568,.T.);
#4740=ORIENTED_EDGE('',*,*,#3556,.F.);
#4741=ORIENTED_EDGE('',*,*,#3568,.F.);
#4742=ORIENTED_EDGE('',*,*,#3569,.F.);
#4743=ORIENTED_EDGE('',*,*,#3570,.T.);
#4744=ORIENTED_EDGE('',*,*,#3557,.F.);
#4745=ORIENTED_EDGE('',*,*,#3570,.F.);
#4746=ORIENTED_EDGE('',*,*,#3571,.F.);
#4747=ORIENTED_EDGE('',*,*,#3572,.T.);
#4748=ORIENTED_EDGE('',*,*,#3558,.F.);
#4749=ORIENTED_EDGE('',*,*,#3572,.F.);
#4750=ORIENTED_EDGE('',*,*,#3573,.F.);
#4751=ORIENTED_EDGE('',*,*,#3574,.F.);
#4752=ORIENTED_EDGE('',*,*,#3571,.T.);
#4753=ORIENTED_EDGE('',*,*,#3569,.T.);
#4754=ORIENTED_EDGE('',*,*,#3567,.T.);
#4755=ORIENTED_EDGE('',*,*,#3565,.T.);
#4756=ORIENTED_EDGE('',*,*,#3563,.T.);
#4757=ORIENTED_EDGE('',*,*,#3561,.T.);
#4758=ORIENTED_EDGE('',*,*,#3552,.F.);
#4759=ORIENTED_EDGE('',*,*,#3575,.T.);
#4760=ORIENTED_EDGE('',*,*,#3573,.T.);
#4761=ORIENTED_EDGE('',*,*,#3575,.F.);
#4762=ORIENTED_EDGE('',*,*,#3574,.T.);
#4763=ORIENTED_EDGE('',*,*,#3576,.T.);
#4764=ORIENTED_EDGE('',*,*,#3577,.T.);
#4765=ORIENTED_EDGE('',*,*,#3576,.F.);
#4766=ORIENTED_EDGE('',*,*,#3577,.F.);
#4767=ORIENTED_EDGE('',*,*,#3542,.T.);
#4768=ORIENTED_EDGE('',*,*,#3560,.F.);
#4769=ORIENTED_EDGE('',*,*,#3549,.T.);
#4770=ORIENTED_EDGE('',*,*,#3546,.T.);
#4771=ORIENTED_EDGE('',*,*,#3578,.F.);
#4772=ORIENTED_EDGE('',*,*,#3579,.T.);
#4773=ORIENTED_EDGE('',*,*,#3580,.T.);
#4774=ORIENTED_EDGE('',*,*,#3579,.F.);
#4775=ORIENTED_EDGE('',*,*,#3581,.F.);
#4776=ORIENTED_EDGE('',*,*,#3582,.T.);
#4777=ORIENTED_EDGE('',*,*,#3583,.T.);
#4778=ORIENTED_EDGE('',*,*,#3582,.F.);
#4779=ORIENTED_EDGE('',*,*,#3581,.T.);
#4780=ORIENTED_EDGE('',*,*,#3578,.T.);
#4781=ORIENTED_EDGE('',*,*,#3583,.F.);
#4782=ORIENTED_EDGE('',*,*,#3580,.F.);
#4783=ORIENTED_EDGE('',*,*,#3584,.F.);
#4784=ORIENTED_EDGE('',*,*,#3585,.T.);
#4785=ORIENTED_EDGE('',*,*,#3586,.F.);
#4786=ORIENTED_EDGE('',*,*,#3587,.F.);
#4787=ORIENTED_EDGE('',*,*,#3588,.F.);
#4788=ORIENTED_EDGE('',*,*,#3589,.T.);
#4789=ORIENTED_EDGE('',*,*,#3590,.F.);
#4790=ORIENTED_EDGE('',*,*,#3585,.F.);
#4791=ORIENTED_EDGE('',*,*,#3591,.F.);
#4792=ORIENTED_EDGE('',*,*,#3592,.F.);
#4793=ORIENTED_EDGE('',*,*,#3593,.F.);
#4794=ORIENTED_EDGE('',*,*,#3594,.F.);
#4795=ORIENTED_EDGE('',*,*,#3589,.F.);
#4796=ORIENTED_EDGE('',*,*,#3595,.T.);
#4797=ORIENTED_EDGE('',*,*,#3586,.T.);
#4798=ORIENTED_EDGE('',*,*,#3590,.T.);
#4799=ORIENTED_EDGE('',*,*,#3594,.T.);
#4800=ORIENTED_EDGE('',*,*,#3596,.T.);
#4801=ORIENTED_EDGE('',*,*,#3587,.T.);
#4802=ORIENTED_EDGE('',*,*,#3596,.F.);
#4803=ORIENTED_EDGE('',*,*,#3593,.T.);
#4804=ORIENTED_EDGE('',*,*,#3597,.F.);
#4805=ORIENTED_EDGE('',*,*,#3598,.T.);
#4806=ORIENTED_EDGE('',*,*,#3599,.T.);
#4807=ORIENTED_EDGE('',*,*,#3600,.T.);
#4808=ORIENTED_EDGE('',*,*,#3601,.T.);
#4809=ORIENTED_EDGE('',*,*,#3602,.T.);
#4810=ORIENTED_EDGE('',*,*,#3603,.T.);
#4811=ORIENTED_EDGE('',*,*,#3604,.F.);
#4812=ORIENTED_EDGE('',*,*,#3605,.F.);
#4813=ORIENTED_EDGE('',*,*,#3606,.F.);
#4814=ORIENTED_EDGE('',*,*,#3607,.T.);
#4815=ORIENTED_EDGE('',*,*,#3600,.F.);
#4816=ORIENTED_EDGE('',*,*,#3601,.F.);
#4817=ORIENTED_EDGE('',*,*,#3607,.F.);
#4818=ORIENTED_EDGE('',*,*,#3602,.F.);
#4819=ORIENTED_EDGE('',*,*,#3603,.F.);
#4820=ORIENTED_EDGE('',*,*,#3608,.T.);
#4821=ORIENTED_EDGE('',*,*,#3609,.F.);
#4822=ORIENTED_EDGE('',*,*,#3610,.F.);
#4823=ORIENTED_EDGE('',*,*,#3611,.F.);
#4824=ORIENTED_EDGE('',*,*,#3608,.F.);
#4825=ORIENTED_EDGE('',*,*,#3612,.F.);
#4826=ORIENTED_EDGE('',*,*,#3613,.T.);
#4827=ORIENTED_EDGE('',*,*,#3605,.T.);
#4828=ORIENTED_EDGE('',*,*,#3614,.T.);
#4829=ORIENTED_EDGE('',*,*,#3615,.F.);
#4830=ORIENTED_EDGE('',*,*,#3614,.F.);
#4831=ORIENTED_EDGE('',*,*,#3604,.T.);
#4832=ORIENTED_EDGE('',*,*,#3606,.T.);
#4833=ORIENTED_EDGE('',*,*,#3613,.F.);
#4834=ORIENTED_EDGE('',*,*,#3610,.T.);
#4835=ORIENTED_EDGE('',*,*,#3609,.T.);
#4836=ORIENTED_EDGE('',*,*,#3611,.T.);
#4837=ORIENTED_EDGE('',*,*,#3616,.T.);
#4838=ORIENTED_EDGE('',*,*,#3617,.T.);
#4839=ORIENTED_EDGE('',*,*,#3618,.T.);
#4840=ORIENTED_EDGE('',*,*,#3619,.T.);
#4841=ORIENTED_EDGE('',*,*,#3620,.T.);
#4842=ORIENTED_EDGE('',*,*,#3621,.T.);
#4843=ORIENTED_EDGE('',*,*,#3617,.F.);
#4844=ORIENTED_EDGE('',*,*,#3616,.F.);
#4845=ORIENTED_EDGE('',*,*,#3618,.F.);
#4846=ORIENTED_EDGE('',*,*,#3622,.T.);
#4847=ORIENTED_EDGE('',*,*,#3591,.T.);
#4848=ORIENTED_EDGE('',*,*,#3622,.F.);
#4849=ORIENTED_EDGE('',*,*,#3598,.F.);
#4850=ORIENTED_EDGE('',*,*,#3599,.F.);
#4851=ORIENTED_EDGE('',*,*,#3623,.T.);
#4852=ORIENTED_EDGE('',*,*,#3620,.F.);
#4853=ORIENTED_EDGE('',*,*,#3619,.F.);
#4854=ORIENTED_EDGE('',*,*,#3621,.F.);
#4855=ORIENTED_EDGE('',*,*,#3623,.F.);
#4856=ORIENTED_EDGE('',*,*,#3612,.T.);
#4857=ORIENTED_EDGE('',*,*,#3584,.T.);
#4858=ORIENTED_EDGE('',*,*,#3597,.T.);
#4859=ORIENTED_EDGE('',*,*,#3592,.T.);
#4860=ORIENTED_EDGE('',*,*,#3588,.T.);
#4861=ORIENTED_EDGE('',*,*,#3624,.T.);
#4862=ORIENTED_EDGE('',*,*,#3625,.T.);
#4863=ORIENTED_EDGE('',*,*,#3626,.F.);
#4864=ORIENTED_EDGE('',*,*,#3627,.T.);
#4865=ORIENTED_EDGE('',*,*,#3628,.F.);
#4866=ORIENTED_EDGE('',*,*,#3629,.T.);
#4867=ORIENTED_EDGE('',*,*,#3630,.F.);
#4868=ORIENTED_EDGE('',*,*,#3631,.T.);
#4869=ORIENTED_EDGE('',*,*,#3632,.F.);
#4870=ORIENTED_EDGE('',*,*,#3633,.T.);
#4871=ORIENTED_EDGE('',*,*,#3634,.F.);
#4872=ORIENTED_EDGE('',*,*,#3635,.T.);
#4873=ORIENTED_EDGE('',*,*,#3636,.F.);
#4874=ORIENTED_EDGE('',*,*,#3637,.T.);
#4875=ORIENTED_EDGE('',*,*,#3638,.F.);
#4876=ORIENTED_EDGE('',*,*,#3639,.T.);
#4877=ORIENTED_EDGE('',*,*,#3640,.F.);
#4878=ORIENTED_EDGE('',*,*,#3641,.T.);
#4879=ORIENTED_EDGE('',*,*,#3642,.F.);
#4880=ORIENTED_EDGE('',*,*,#3643,.T.);
#4881=ORIENTED_EDGE('',*,*,#3644,.F.);
#4882=ORIENTED_EDGE('',*,*,#3645,.T.);
#4883=ORIENTED_EDGE('',*,*,#3646,.F.);
#4884=ORIENTED_EDGE('',*,*,#3647,.T.);
#4885=ORIENTED_EDGE('',*,*,#3648,.F.);
#4886=ORIENTED_EDGE('',*,*,#3649,.T.);
#4887=ORIENTED_EDGE('',*,*,#3650,.F.);
#4888=ORIENTED_EDGE('',*,*,#3651,.T.);
#4889=ORIENTED_EDGE('',*,*,#3652,.F.);
#4890=ORIENTED_EDGE('',*,*,#3653,.T.);
#4891=ORIENTED_EDGE('',*,*,#3654,.F.);
#4892=ORIENTED_EDGE('',*,*,#3655,.T.);
#4893=ORIENTED_EDGE('',*,*,#3656,.F.);
#4894=ORIENTED_EDGE('',*,*,#3657,.T.);
#4895=ORIENTED_EDGE('',*,*,#3658,.F.);
#4896=ORIENTED_EDGE('',*,*,#3659,.T.);
#4897=ORIENTED_EDGE('',*,*,#3660,.F.);
#4898=ORIENTED_EDGE('',*,*,#3661,.T.);
#4899=ORIENTED_EDGE('',*,*,#3662,.F.);
#4900=ORIENTED_EDGE('',*,*,#3663,.T.);
#4901=ORIENTED_EDGE('',*,*,#3664,.F.);
#4902=ORIENTED_EDGE('',*,*,#3665,.T.);
#4903=ORIENTED_EDGE('',*,*,#3666,.F.);
#4904=ORIENTED_EDGE('',*,*,#3667,.T.);
#4905=ORIENTED_EDGE('',*,*,#3668,.F.);
#4906=ORIENTED_EDGE('',*,*,#3669,.T.);
#4907=ORIENTED_EDGE('',*,*,#3670,.F.);
#4908=ORIENTED_EDGE('',*,*,#3671,.T.);
#4909=ORIENTED_EDGE('',*,*,#3672,.F.);
#4910=ORIENTED_EDGE('',*,*,#3673,.T.);
#4911=ORIENTED_EDGE('',*,*,#3674,.F.);
#4912=ORIENTED_EDGE('',*,*,#3675,.T.);
#4913=ORIENTED_EDGE('',*,*,#3676,.F.);
#4914=ORIENTED_EDGE('',*,*,#3677,.T.);
#4915=ORIENTED_EDGE('',*,*,#3678,.F.);
#4916=ORIENTED_EDGE('',*,*,#3679,.T.);
#4917=ORIENTED_EDGE('',*,*,#3680,.F.);
#4918=ORIENTED_EDGE('',*,*,#3681,.T.);
#4919=ORIENTED_EDGE('',*,*,#3682,.F.);
#4920=ORIENTED_EDGE('',*,*,#3683,.T.);
#4921=ORIENTED_EDGE('',*,*,#3684,.F.);
#4922=ORIENTED_EDGE('',*,*,#3685,.T.);
#4923=ORIENTED_EDGE('',*,*,#3686,.F.);
#4924=ORIENTED_EDGE('',*,*,#3687,.T.);
#4925=ORIENTED_EDGE('',*,*,#3688,.F.);
#4926=ORIENTED_EDGE('',*,*,#3689,.T.);
#4927=ORIENTED_EDGE('',*,*,#3690,.F.);
#4928=ORIENTED_EDGE('',*,*,#3691,.T.);
#4929=ORIENTED_EDGE('',*,*,#3692,.F.);
#4930=ORIENTED_EDGE('',*,*,#3693,.T.);
#4931=ORIENTED_EDGE('',*,*,#3694,.F.);
#4932=ORIENTED_EDGE('',*,*,#3695,.T.);
#4933=ORIENTED_EDGE('',*,*,#3696,.F.);
#4934=ORIENTED_EDGE('',*,*,#3697,.T.);
#4935=ORIENTED_EDGE('',*,*,#3698,.F.);
#4936=ORIENTED_EDGE('',*,*,#3699,.T.);
#4937=ORIENTED_EDGE('',*,*,#3700,.F.);
#4938=ORIENTED_EDGE('',*,*,#3701,.T.);
#4939=ORIENTED_EDGE('',*,*,#3702,.F.);
#4940=ORIENTED_EDGE('',*,*,#3703,.T.);
#4941=ORIENTED_EDGE('',*,*,#3704,.F.);
#4942=ORIENTED_EDGE('',*,*,#3705,.F.);
#4943=ORIENTED_EDGE('',*,*,#3706,.T.);
#4944=ORIENTED_EDGE('',*,*,#3624,.F.);
#4945=ORIENTED_EDGE('',*,*,#3706,.F.);
#4946=ORIENTED_EDGE('',*,*,#3705,.T.);
#4947=ORIENTED_EDGE('',*,*,#3615,.T.);
#4948=ORIENTED_EDGE('',*,*,#3707,.F.);
#4949=ORIENTED_EDGE('',*,*,#3708,.T.);
#4950=ORIENTED_EDGE('',*,*,#3709,.T.);
#4951=ORIENTED_EDGE('',*,*,#3710,.T.);
#4952=ORIENTED_EDGE('',*,*,#3711,.T.);
#4953=ORIENTED_EDGE('',*,*,#3712,.T.);
#4954=ORIENTED_EDGE('',*,*,#3713,.T.);
#4955=ORIENTED_EDGE('',*,*,#3714,.T.);
#4956=ORIENTED_EDGE('',*,*,#3715,.T.);
#4957=ORIENTED_EDGE('',*,*,#3716,.T.);
#4958=ORIENTED_EDGE('',*,*,#3717,.T.);
#4959=ORIENTED_EDGE('',*,*,#3718,.T.);
#4960=ORIENTED_EDGE('',*,*,#3719,.T.);
#4961=ORIENTED_EDGE('',*,*,#3720,.T.);
#4962=ORIENTED_EDGE('',*,*,#3721,.T.);
#4963=ORIENTED_EDGE('',*,*,#3722,.T.);
#4964=ORIENTED_EDGE('',*,*,#3723,.T.);
#4965=ORIENTED_EDGE('',*,*,#3724,.T.);
#4966=ORIENTED_EDGE('',*,*,#3725,.T.);
#4967=ORIENTED_EDGE('',*,*,#3726,.T.);
#4968=ORIENTED_EDGE('',*,*,#3727,.T.);
#4969=ORIENTED_EDGE('',*,*,#3728,.T.);
#4970=ORIENTED_EDGE('',*,*,#3729,.T.);
#4971=ORIENTED_EDGE('',*,*,#3730,.T.);
#4972=ORIENTED_EDGE('',*,*,#3731,.T.);
#4973=ORIENTED_EDGE('',*,*,#3732,.T.);
#4974=ORIENTED_EDGE('',*,*,#3733,.T.);
#4975=ORIENTED_EDGE('',*,*,#3734,.T.);
#4976=ORIENTED_EDGE('',*,*,#3735,.T.);
#4977=ORIENTED_EDGE('',*,*,#3736,.T.);
#4978=ORIENTED_EDGE('',*,*,#3737,.T.);
#4979=ORIENTED_EDGE('',*,*,#3738,.T.);
#4980=ORIENTED_EDGE('',*,*,#3739,.T.);
#4981=ORIENTED_EDGE('',*,*,#3740,.T.);
#4982=ORIENTED_EDGE('',*,*,#3741,.T.);
#4983=ORIENTED_EDGE('',*,*,#3742,.T.);
#4984=ORIENTED_EDGE('',*,*,#3743,.T.);
#4985=ORIENTED_EDGE('',*,*,#3744,.T.);
#4986=ORIENTED_EDGE('',*,*,#3745,.T.);
#4987=ORIENTED_EDGE('',*,*,#3746,.T.);
#4988=ORIENTED_EDGE('',*,*,#3747,.T.);
#4989=ORIENTED_EDGE('',*,*,#3748,.T.);
#4990=ORIENTED_EDGE('',*,*,#3749,.T.);
#4991=ORIENTED_EDGE('',*,*,#3750,.T.);
#4992=ORIENTED_EDGE('',*,*,#3751,.T.);
#4993=ORIENTED_EDGE('',*,*,#3752,.T.);
#4994=ORIENTED_EDGE('',*,*,#3753,.T.);
#4995=ORIENTED_EDGE('',*,*,#3754,.T.);
#4996=ORIENTED_EDGE('',*,*,#3755,.T.);
#4997=ORIENTED_EDGE('',*,*,#3756,.T.);
#4998=ORIENTED_EDGE('',*,*,#3757,.T.);
#4999=ORIENTED_EDGE('',*,*,#3758,.T.);
#5000=ORIENTED_EDGE('',*,*,#3759,.T.);
#5001=ORIENTED_EDGE('',*,*,#3760,.T.);
#5002=ORIENTED_EDGE('',*,*,#3761,.T.);
#5003=ORIENTED_EDGE('',*,*,#3762,.T.);
#5004=ORIENTED_EDGE('',*,*,#3763,.T.);
#5005=ORIENTED_EDGE('',*,*,#3764,.T.);
#5006=ORIENTED_EDGE('',*,*,#3765,.T.);
#5007=ORIENTED_EDGE('',*,*,#3766,.T.);
#5008=ORIENTED_EDGE('',*,*,#3767,.T.);
#5009=ORIENTED_EDGE('',*,*,#3768,.T.);
#5010=ORIENTED_EDGE('',*,*,#3769,.T.);
#5011=ORIENTED_EDGE('',*,*,#3770,.T.);
#5012=ORIENTED_EDGE('',*,*,#3771,.T.);
#5013=ORIENTED_EDGE('',*,*,#3772,.T.);
#5014=ORIENTED_EDGE('',*,*,#3773,.T.);
#5015=ORIENTED_EDGE('',*,*,#3774,.T.);
#5016=ORIENTED_EDGE('',*,*,#3775,.T.);
#5017=ORIENTED_EDGE('',*,*,#3776,.T.);
#5018=ORIENTED_EDGE('',*,*,#3777,.T.);
#5019=ORIENTED_EDGE('',*,*,#3778,.T.);
#5020=ORIENTED_EDGE('',*,*,#3779,.T.);
#5021=ORIENTED_EDGE('',*,*,#3780,.T.);
#5022=ORIENTED_EDGE('',*,*,#3781,.T.);
#5023=ORIENTED_EDGE('',*,*,#3782,.T.);
#5024=ORIENTED_EDGE('',*,*,#3783,.T.);
#5025=ORIENTED_EDGE('',*,*,#3784,.T.);
#5026=ORIENTED_EDGE('',*,*,#3785,.T.);
#5027=ORIENTED_EDGE('',*,*,#3786,.T.);
#5028=ORIENTED_EDGE('',*,*,#3787,.T.);
#5029=ORIENTED_EDGE('',*,*,#3595,.F.);
#5030=ORIENTED_EDGE('',*,*,#3788,.T.);
#5031=ORIENTED_EDGE('',*,*,#3707,.T.);
#5032=ORIENTED_EDGE('',*,*,#3788,.F.);
#5033=ORIENTED_EDGE('',*,*,#3789,.F.);
#5034=ORIENTED_EDGE('',*,*,#3708,.F.);
#5035=ORIENTED_EDGE('',*,*,#3790,.F.);
#5036=ORIENTED_EDGE('',*,*,#3625,.F.);
#5037=ORIENTED_EDGE('',*,*,#3790,.T.);
#5038=ORIENTED_EDGE('',*,*,#3787,.F.);
#5039=ORIENTED_EDGE('',*,*,#3791,.T.);
#5040=ORIENTED_EDGE('',*,*,#3626,.T.);
#5041=ORIENTED_EDGE('',*,*,#3791,.F.);
#5042=ORIENTED_EDGE('',*,*,#3786,.F.);
#5043=ORIENTED_EDGE('',*,*,#3792,.F.);
#5044=ORIENTED_EDGE('',*,*,#3627,.F.);
#5045=ORIENTED_EDGE('',*,*,#3792,.T.);
#5046=ORIENTED_EDGE('',*,*,#3785,.F.);
#5047=ORIENTED_EDGE('',*,*,#3793,.T.);
#5048=ORIENTED_EDGE('',*,*,#3628,.T.);
#5049=ORIENTED_EDGE('',*,*,#3793,.F.);
#5050=ORIENTED_EDGE('',*,*,#3784,.F.);
#5051=ORIENTED_EDGE('',*,*,#3794,.F.);
#5052=ORIENTED_EDGE('',*,*,#3629,.F.);
#5053=ORIENTED_EDGE('',*,*,#3794,.T.);
#5054=ORIENTED_EDGE('',*,*,#3783,.F.);
#5055=ORIENTED_EDGE('',*,*,#3795,.T.);
#5056=ORIENTED_EDGE('',*,*,#3630,.T.);
#5057=ORIENTED_EDGE('',*,*,#3795,.F.);
#5058=ORIENTED_EDGE('',*,*,#3782,.F.);
#5059=ORIENTED_EDGE('',*,*,#3796,.F.);
#5060=ORIENTED_EDGE('',*,*,#3631,.F.);
#5061=ORIENTED_EDGE('',*,*,#3796,.T.);
#5062=ORIENTED_EDGE('',*,*,#3781,.F.);
#5063=ORIENTED_EDGE('',*,*,#3797,.T.);
#5064=ORIENTED_EDGE('',*,*,#3632,.T.);
#5065=ORIENTED_EDGE('',*,*,#3797,.F.);
#5066=ORIENTED_EDGE('',*,*,#3780,.F.);
#5067=ORIENTED_EDGE('',*,*,#3798,.F.);
#5068=ORIENTED_EDGE('',*,*,#3633,.F.);
#5069=ORIENTED_EDGE('',*,*,#3798,.T.);
#5070=ORIENTED_EDGE('',*,*,#3779,.F.);
#5071=ORIENTED_EDGE('',*,*,#3799,.T.);
#5072=ORIENTED_EDGE('',*,*,#3634,.T.);
#5073=ORIENTED_EDGE('',*,*,#3799,.F.);
#5074=ORIENTED_EDGE('',*,*,#3778,.F.);
#5075=ORIENTED_EDGE('',*,*,#3800,.F.);
#5076=ORIENTED_EDGE('',*,*,#3635,.F.);
#5077=ORIENTED_EDGE('',*,*,#3800,.T.);
#5078=ORIENTED_EDGE('',*,*,#3777,.F.);
#5079=ORIENTED_EDGE('',*,*,#3801,.T.);
#5080=ORIENTED_EDGE('',*,*,#3636,.T.);
#5081=ORIENTED_EDGE('',*,*,#3801,.F.);
#5082=ORIENTED_EDGE('',*,*,#3776,.F.);
#5083=ORIENTED_EDGE('',*,*,#3802,.F.);
#5084=ORIENTED_EDGE('',*,*,#3637,.F.);
#5085=ORIENTED_EDGE('',*,*,#3802,.T.);
#5086=ORIENTED_EDGE('',*,*,#3775,.F.);
#5087=ORIENTED_EDGE('',*,*,#3803,.T.);
#5088=ORIENTED_EDGE('',*,*,#3638,.T.);
#5089=ORIENTED_EDGE('',*,*,#3803,.F.);
#5090=ORIENTED_EDGE('',*,*,#3774,.F.);
#5091=ORIENTED_EDGE('',*,*,#3804,.F.);
#5092=ORIENTED_EDGE('',*,*,#3639,.F.);
#5093=ORIENTED_EDGE('',*,*,#3804,.T.);
#5094=ORIENTED_EDGE('',*,*,#3773,.F.);
#5095=ORIENTED_EDGE('',*,*,#3805,.T.);
#5096=ORIENTED_EDGE('',*,*,#3640,.T.);
#5097=ORIENTED_EDGE('',*,*,#3805,.F.);
#5098=ORIENTED_EDGE('',*,*,#3772,.F.);
#5099=ORIENTED_EDGE('',*,*,#3806,.F.);
#5100=ORIENTED_EDGE('',*,*,#3641,.F.);
#5101=ORIENTED_EDGE('',*,*,#3806,.T.);
#5102=ORIENTED_EDGE('',*,*,#3771,.F.);
#5103=ORIENTED_EDGE('',*,*,#3807,.T.);
#5104=ORIENTED_EDGE('',*,*,#3642,.T.);
#5105=ORIENTED_EDGE('',*,*,#3807,.F.);
#5106=ORIENTED_EDGE('',*,*,#3770,.F.);
#5107=ORIENTED_EDGE('',*,*,#3808,.F.);
#5108=ORIENTED_EDGE('',*,*,#3643,.F.);
#5109=ORIENTED_EDGE('',*,*,#3808,.T.);
#5110=ORIENTED_EDGE('',*,*,#3769,.F.);
#5111=ORIENTED_EDGE('',*,*,#3809,.T.);
#5112=ORIENTED_EDGE('',*,*,#3644,.T.);
#5113=ORIENTED_EDGE('',*,*,#3809,.F.);
#5114=ORIENTED_EDGE('',*,*,#3768,.F.);
#5115=ORIENTED_EDGE('',*,*,#3810,.F.);
#5116=ORIENTED_EDGE('',*,*,#3645,.F.);
#5117=ORIENTED_EDGE('',*,*,#3810,.T.);
#5118=ORIENTED_EDGE('',*,*,#3767,.F.);
#5119=ORIENTED_EDGE('',*,*,#3811,.T.);
#5120=ORIENTED_EDGE('',*,*,#3646,.T.);
#5121=ORIENTED_EDGE('',*,*,#3811,.F.);
#5122=ORIENTED_EDGE('',*,*,#3766,.F.);
#5123=ORIENTED_EDGE('',*,*,#3812,.F.);
#5124=ORIENTED_EDGE('',*,*,#3647,.F.);
#5125=ORIENTED_EDGE('',*,*,#3812,.T.);
#5126=ORIENTED_EDGE('',*,*,#3765,.F.);
#5127=ORIENTED_EDGE('',*,*,#3813,.T.);
#5128=ORIENTED_EDGE('',*,*,#3648,.T.);
#5129=ORIENTED_EDGE('',*,*,#3813,.F.);
#5130=ORIENTED_EDGE('',*,*,#3764,.F.);
#5131=ORIENTED_EDGE('',*,*,#3814,.F.);
#5132=ORIENTED_EDGE('',*,*,#3649,.F.);
#5133=ORIENTED_EDGE('',*,*,#3814,.T.);
#5134=ORIENTED_EDGE('',*,*,#3763,.F.);
#5135=ORIENTED_EDGE('',*,*,#3815,.T.);
#5136=ORIENTED_EDGE('',*,*,#3650,.T.);
#5137=ORIENTED_EDGE('',*,*,#3815,.F.);
#5138=ORIENTED_EDGE('',*,*,#3762,.F.);
#5139=ORIENTED_EDGE('',*,*,#3816,.F.);
#5140=ORIENTED_EDGE('',*,*,#3651,.F.);
#5141=ORIENTED_EDGE('',*,*,#3816,.T.);
#5142=ORIENTED_EDGE('',*,*,#3761,.F.);
#5143=ORIENTED_EDGE('',*,*,#3817,.T.);
#5144=ORIENTED_EDGE('',*,*,#3652,.T.);
#5145=ORIENTED_EDGE('',*,*,#3817,.F.);
#5146=ORIENTED_EDGE('',*,*,#3760,.F.);
#5147=ORIENTED_EDGE('',*,*,#3818,.F.);
#5148=ORIENTED_EDGE('',*,*,#3653,.F.);
#5149=ORIENTED_EDGE('',*,*,#3818,.T.);
#5150=ORIENTED_EDGE('',*,*,#3759,.F.);
#5151=ORIENTED_EDGE('',*,*,#3819,.T.);
#5152=ORIENTED_EDGE('',*,*,#3654,.T.);
#5153=ORIENTED_EDGE('',*,*,#3819,.F.);
#5154=ORIENTED_EDGE('',*,*,#3758,.F.);
#5155=ORIENTED_EDGE('',*,*,#3820,.F.);
#5156=ORIENTED_EDGE('',*,*,#3655,.F.);
#5157=ORIENTED_EDGE('',*,*,#3820,.T.);
#5158=ORIENTED_EDGE('',*,*,#3757,.F.);
#5159=ORIENTED_EDGE('',*,*,#3821,.T.);
#5160=ORIENTED_EDGE('',*,*,#3656,.T.);
#5161=ORIENTED_EDGE('',*,*,#3821,.F.);
#5162=ORIENTED_EDGE('',*,*,#3756,.F.);
#5163=ORIENTED_EDGE('',*,*,#3822,.F.);
#5164=ORIENTED_EDGE('',*,*,#3657,.F.);
#5165=ORIENTED_EDGE('',*,*,#3822,.T.);
#5166=ORIENTED_EDGE('',*,*,#3755,.F.);
#5167=ORIENTED_EDGE('',*,*,#3823,.T.);
#5168=ORIENTED_EDGE('',*,*,#3658,.T.);
#5169=ORIENTED_EDGE('',*,*,#3823,.F.);
#5170=ORIENTED_EDGE('',*,*,#3754,.F.);
#5171=ORIENTED_EDGE('',*,*,#3824,.F.);
#5172=ORIENTED_EDGE('',*,*,#3659,.F.);
#5173=ORIENTED_EDGE('',*,*,#3824,.T.);
#5174=ORIENTED_EDGE('',*,*,#3753,.F.);
#5175=ORIENTED_EDGE('',*,*,#3825,.T.);
#5176=ORIENTED_EDGE('',*,*,#3660,.T.);
#5177=ORIENTED_EDGE('',*,*,#3825,.F.);
#5178=ORIENTED_EDGE('',*,*,#3752,.F.);
#5179=ORIENTED_EDGE('',*,*,#3826,.F.);
#5180=ORIENTED_EDGE('',*,*,#3661,.F.);
#5181=ORIENTED_EDGE('',*,*,#3826,.T.);
#5182=ORIENTED_EDGE('',*,*,#3751,.F.);
#5183=ORIENTED_EDGE('',*,*,#3827,.T.);
#5184=ORIENTED_EDGE('',*,*,#3662,.T.);
#5185=ORIENTED_EDGE('',*,*,#3827,.F.);
#5186=ORIENTED_EDGE('',*,*,#3750,.F.);
#5187=ORIENTED_EDGE('',*,*,#3828,.F.);
#5188=ORIENTED_EDGE('',*,*,#3663,.F.);
#5189=ORIENTED_EDGE('',*,*,#3828,.T.);
#5190=ORIENTED_EDGE('',*,*,#3749,.F.);
#5191=ORIENTED_EDGE('',*,*,#3829,.T.);
#5192=ORIENTED_EDGE('',*,*,#3664,.T.);
#5193=ORIENTED_EDGE('',*,*,#3829,.F.);
#5194=ORIENTED_EDGE('',*,*,#3748,.F.);
#5195=ORIENTED_EDGE('',*,*,#3830,.F.);
#5196=ORIENTED_EDGE('',*,*,#3665,.F.);
#5197=ORIENTED_EDGE('',*,*,#3830,.T.);
#5198=ORIENTED_EDGE('',*,*,#3747,.F.);
#5199=ORIENTED_EDGE('',*,*,#3831,.T.);
#5200=ORIENTED_EDGE('',*,*,#3666,.T.);
#5201=ORIENTED_EDGE('',*,*,#3831,.F.);
#5202=ORIENTED_EDGE('',*,*,#3746,.F.);
#5203=ORIENTED_EDGE('',*,*,#3832,.F.);
#5204=ORIENTED_EDGE('',*,*,#3667,.F.);
#5205=ORIENTED_EDGE('',*,*,#3832,.T.);
#5206=ORIENTED_EDGE('',*,*,#3745,.F.);
#5207=ORIENTED_EDGE('',*,*,#3833,.T.);
#5208=ORIENTED_EDGE('',*,*,#3668,.T.);
#5209=ORIENTED_EDGE('',*,*,#3833,.F.);
#5210=ORIENTED_EDGE('',*,*,#3744,.F.);
#5211=ORIENTED_EDGE('',*,*,#3834,.F.);
#5212=ORIENTED_EDGE('',*,*,#3669,.F.);
#5213=ORIENTED_EDGE('',*,*,#3834,.T.);
#5214=ORIENTED_EDGE('',*,*,#3743,.F.);
#5215=ORIENTED_EDGE('',*,*,#3835,.T.);
#5216=ORIENTED_EDGE('',*,*,#3670,.T.);
#5217=ORIENTED_EDGE('',*,*,#3835,.F.);
#5218=ORIENTED_EDGE('',*,*,#3742,.F.);
#5219=ORIENTED_EDGE('',*,*,#3836,.F.);
#5220=ORIENTED_EDGE('',*,*,#3671,.F.);
#5221=ORIENTED_EDGE('',*,*,#3836,.T.);
#5222=ORIENTED_EDGE('',*,*,#3741,.F.);
#5223=ORIENTED_EDGE('',*,*,#3837,.T.);
#5224=ORIENTED_EDGE('',*,*,#3672,.T.);
#5225=ORIENTED_EDGE('',*,*,#3837,.F.);
#5226=ORIENTED_EDGE('',*,*,#3740,.F.);
#5227=ORIENTED_EDGE('',*,*,#3838,.F.);
#5228=ORIENTED_EDGE('',*,*,#3673,.F.);
#5229=ORIENTED_EDGE('',*,*,#3838,.T.);
#5230=ORIENTED_EDGE('',*,*,#3739,.F.);
#5231=ORIENTED_EDGE('',*,*,#3839,.T.);
#5232=ORIENTED_EDGE('',*,*,#3674,.T.);
#5233=ORIENTED_EDGE('',*,*,#3839,.F.);
#5234=ORIENTED_EDGE('',*,*,#3738,.F.);
#5235=ORIENTED_EDGE('',*,*,#3840,.F.);
#5236=ORIENTED_EDGE('',*,*,#3675,.F.);
#5237=ORIENTED_EDGE('',*,*,#3840,.T.);
#5238=ORIENTED_EDGE('',*,*,#3737,.F.);
#5239=ORIENTED_EDGE('',*,*,#3841,.T.);
#5240=ORIENTED_EDGE('',*,*,#3676,.T.);
#5241=ORIENTED_EDGE('',*,*,#3841,.F.);
#5242=ORIENTED_EDGE('',*,*,#3736,.F.);
#5243=ORIENTED_EDGE('',*,*,#3842,.F.);
#5244=ORIENTED_EDGE('',*,*,#3677,.F.);
#5245=ORIENTED_EDGE('',*,*,#3842,.T.);
#5246=ORIENTED_EDGE('',*,*,#3735,.F.);
#5247=ORIENTED_EDGE('',*,*,#3843,.T.);
#5248=ORIENTED_EDGE('',*,*,#3678,.T.);
#5249=ORIENTED_EDGE('',*,*,#3843,.F.);
#5250=ORIENTED_EDGE('',*,*,#3734,.F.);
#5251=ORIENTED_EDGE('',*,*,#3844,.F.);
#5252=ORIENTED_EDGE('',*,*,#3679,.F.);
#5253=ORIENTED_EDGE('',*,*,#3844,.T.);
#5254=ORIENTED_EDGE('',*,*,#3733,.F.);
#5255=ORIENTED_EDGE('',*,*,#3845,.T.);
#5256=ORIENTED_EDGE('',*,*,#3680,.T.);
#5257=ORIENTED_EDGE('',*,*,#3845,.F.);
#5258=ORIENTED_EDGE('',*,*,#3732,.F.);
#5259=ORIENTED_EDGE('',*,*,#3846,.F.);
#5260=ORIENTED_EDGE('',*,*,#3681,.F.);
#5261=ORIENTED_EDGE('',*,*,#3846,.T.);
#5262=ORIENTED_EDGE('',*,*,#3731,.F.);
#5263=ORIENTED_EDGE('',*,*,#3847,.T.);
#5264=ORIENTED_EDGE('',*,*,#3682,.T.);
#5265=ORIENTED_EDGE('',*,*,#3847,.F.);
#5266=ORIENTED_EDGE('',*,*,#3730,.F.);
#5267=ORIENTED_EDGE('',*,*,#3848,.F.);
#5268=ORIENTED_EDGE('',*,*,#3683,.F.);
#5269=ORIENTED_EDGE('',*,*,#3848,.T.);
#5270=ORIENTED_EDGE('',*,*,#3729,.F.);
#5271=ORIENTED_EDGE('',*,*,#3849,.T.);
#5272=ORIENTED_EDGE('',*,*,#3684,.T.);
#5273=ORIENTED_EDGE('',*,*,#3849,.F.);
#5274=ORIENTED_EDGE('',*,*,#3728,.F.);
#5275=ORIENTED_EDGE('',*,*,#3850,.F.);
#5276=ORIENTED_EDGE('',*,*,#3685,.F.);
#5277=ORIENTED_EDGE('',*,*,#3850,.T.);
#5278=ORIENTED_EDGE('',*,*,#3727,.F.);
#5279=ORIENTED_EDGE('',*,*,#3851,.T.);
#5280=ORIENTED_EDGE('',*,*,#3686,.T.);
#5281=ORIENTED_EDGE('',*,*,#3851,.F.);
#5282=ORIENTED_EDGE('',*,*,#3726,.F.);
#5283=ORIENTED_EDGE('',*,*,#3852,.F.);
#5284=ORIENTED_EDGE('',*,*,#3687,.F.);
#5285=ORIENTED_EDGE('',*,*,#3852,.T.);
#5286=ORIENTED_EDGE('',*,*,#3725,.F.);
#5287=ORIENTED_EDGE('',*,*,#3853,.T.);
#5288=ORIENTED_EDGE('',*,*,#3688,.T.);
#5289=ORIENTED_EDGE('',*,*,#3853,.F.);
#5290=ORIENTED_EDGE('',*,*,#3724,.F.);
#5291=ORIENTED_EDGE('',*,*,#3854,.F.);
#5292=ORIENTED_EDGE('',*,*,#3689,.F.);
#5293=ORIENTED_EDGE('',*,*,#3854,.T.);
#5294=ORIENTED_EDGE('',*,*,#3723,.F.);
#5295=ORIENTED_EDGE('',*,*,#3855,.T.);
#5296=ORIENTED_EDGE('',*,*,#3690,.T.);
#5297=ORIENTED_EDGE('',*,*,#3855,.F.);
#5298=ORIENTED_EDGE('',*,*,#3722,.F.);
#5299=ORIENTED_EDGE('',*,*,#3856,.F.);
#5300=ORIENTED_EDGE('',*,*,#3691,.F.);
#5301=ORIENTED_EDGE('',*,*,#3856,.T.);
#5302=ORIENTED_EDGE('',*,*,#3721,.F.);
#5303=ORIENTED_EDGE('',*,*,#3857,.T.);
#5304=ORIENTED_EDGE('',*,*,#3692,.T.);
#5305=ORIENTED_EDGE('',*,*,#3857,.F.);
#5306=ORIENTED_EDGE('',*,*,#3720,.F.);
#5307=ORIENTED_EDGE('',*,*,#3858,.F.);
#5308=ORIENTED_EDGE('',*,*,#3693,.F.);
#5309=ORIENTED_EDGE('',*,*,#3858,.T.);
#5310=ORIENTED_EDGE('',*,*,#3719,.F.);
#5311=ORIENTED_EDGE('',*,*,#3859,.T.);
#5312=ORIENTED_EDGE('',*,*,#3694,.T.);
#5313=ORIENTED_EDGE('',*,*,#3859,.F.);
#5314=ORIENTED_EDGE('',*,*,#3718,.F.);
#5315=ORIENTED_EDGE('',*,*,#3860,.F.);
#5316=ORIENTED_EDGE('',*,*,#3695,.F.);
#5317=ORIENTED_EDGE('',*,*,#3860,.T.);
#5318=ORIENTED_EDGE('',*,*,#3717,.F.);
#5319=ORIENTED_EDGE('',*,*,#3861,.T.);
#5320=ORIENTED_EDGE('',*,*,#3696,.T.);
#5321=ORIENTED_EDGE('',*,*,#3861,.F.);
#5322=ORIENTED_EDGE('',*,*,#3716,.F.);
#5323=ORIENTED_EDGE('',*,*,#3862,.F.);
#5324=ORIENTED_EDGE('',*,*,#3697,.F.);
#5325=ORIENTED_EDGE('',*,*,#3862,.T.);
#5326=ORIENTED_EDGE('',*,*,#3715,.F.);
#5327=ORIENTED_EDGE('',*,*,#3863,.T.);
#5328=ORIENTED_EDGE('',*,*,#3698,.T.);
#5329=ORIENTED_EDGE('',*,*,#3863,.F.);
#5330=ORIENTED_EDGE('',*,*,#3714,.F.);
#5331=ORIENTED_EDGE('',*,*,#3864,.F.);
#5332=ORIENTED_EDGE('',*,*,#3699,.F.);
#5333=ORIENTED_EDGE('',*,*,#3864,.T.);
#5334=ORIENTED_EDGE('',*,*,#3713,.F.);
#5335=ORIENTED_EDGE('',*,*,#3865,.T.);
#5336=ORIENTED_EDGE('',*,*,#3700,.T.);
#5337=ORIENTED_EDGE('',*,*,#3866,.F.);
#5338=ORIENTED_EDGE('',*,*,#3701,.F.);
#5339=ORIENTED_EDGE('',*,*,#3865,.F.);
#5340=ORIENTED_EDGE('',*,*,#3712,.F.);
#5341=ORIENTED_EDGE('',*,*,#3789,.T.);
#5342=ORIENTED_EDGE('',*,*,#3704,.T.);
#5343=ORIENTED_EDGE('',*,*,#3867,.T.);
#5344=ORIENTED_EDGE('',*,*,#3709,.F.);
#5345=ORIENTED_EDGE('',*,*,#3868,.F.);
#5346=ORIENTED_EDGE('',*,*,#3710,.F.);
#5347=ORIENTED_EDGE('',*,*,#3867,.F.);
#5348=ORIENTED_EDGE('',*,*,#3703,.F.);
#5349=ORIENTED_EDGE('',*,*,#3866,.T.);
#5350=ORIENTED_EDGE('',*,*,#3711,.F.);
#5351=ORIENTED_EDGE('',*,*,#3868,.T.);
#5352=ORIENTED_EDGE('',*,*,#3702,.T.);
#5353=ORIENTED_EDGE('',*,*,#3869,.F.);
#5354=ORIENTED_EDGE('',*,*,#3870,.F.);
#5355=ORIENTED_EDGE('',*,*,#3871,.F.);
#5356=ORIENTED_EDGE('',*,*,#3872,.F.);
#5357=ORIENTED_EDGE('',*,*,#3873,.F.);
#5358=ORIENTED_EDGE('',*,*,#3874,.F.);
#5359=ORIENTED_EDGE('',*,*,#3875,.F.);
#5360=ORIENTED_EDGE('',*,*,#3876,.F.);
#5361=ORIENTED_EDGE('',*,*,#3873,.T.);
#5362=ORIENTED_EDGE('',*,*,#3877,.T.);
#5363=ORIENTED_EDGE('',*,*,#3878,.T.);
#5364=ORIENTED_EDGE('',*,*,#3879,.T.);
#5365=ORIENTED_EDGE('',*,*,#3872,.T.);
#5366=ORIENTED_EDGE('',*,*,#3880,.F.);
#5367=ORIENTED_EDGE('',*,*,#3881,.T.);
#5368=ORIENTED_EDGE('',*,*,#3877,.F.);
#5369=ORIENTED_EDGE('',*,*,#3871,.T.);
#5370=ORIENTED_EDGE('',*,*,#3882,.T.);
#5371=ORIENTED_EDGE('',*,*,#3883,.T.);
#5372=ORIENTED_EDGE('',*,*,#3880,.T.);
#5373=ORIENTED_EDGE('',*,*,#3870,.T.);
#5374=ORIENTED_EDGE('',*,*,#3884,.F.);
#5375=ORIENTED_EDGE('',*,*,#3885,.T.);
#5376=ORIENTED_EDGE('',*,*,#3882,.F.);
#5377=ORIENTED_EDGE('',*,*,#3878,.F.);
#5378=ORIENTED_EDGE('',*,*,#3881,.F.);
#5379=ORIENTED_EDGE('',*,*,#3883,.F.);
#5380=ORIENTED_EDGE('',*,*,#3885,.F.);
#5381=ORIENTED_EDGE('',*,*,#3886,.F.);
#5382=ORIENTED_EDGE('',*,*,#3887,.F.);
#5383=ORIENTED_EDGE('',*,*,#3888,.F.);
#5384=ORIENTED_EDGE('',*,*,#3889,.F.);
#5385=ORIENTED_EDGE('',*,*,#3869,.T.);
#5386=ORIENTED_EDGE('',*,*,#3890,.T.);
#5387=ORIENTED_EDGE('',*,*,#3886,.T.);
#5388=ORIENTED_EDGE('',*,*,#3884,.T.);
#5389=ORIENTED_EDGE('',*,*,#3876,.T.);
#5390=ORIENTED_EDGE('',*,*,#3891,.F.);
#5391=ORIENTED_EDGE('',*,*,#3887,.T.);
#5392=ORIENTED_EDGE('',*,*,#3890,.F.);
#5393=ORIENTED_EDGE('',*,*,#3875,.T.);
#5394=ORIENTED_EDGE('',*,*,#3892,.T.);
#5395=ORIENTED_EDGE('',*,*,#3888,.T.);
#5396=ORIENTED_EDGE('',*,*,#3891,.T.);
#5397=ORIENTED_EDGE('',*,*,#3874,.T.);
#5398=ORIENTED_EDGE('',*,*,#3879,.F.);
#5399=ORIENTED_EDGE('',*,*,#3889,.T.);
#5400=ORIENTED_EDGE('',*,*,#3892,.F.);
#5401=ORIENTED_EDGE('',*,*,#3893,.F.);
#5402=ORIENTED_EDGE('',*,*,#3894,.F.);
#5403=ORIENTED_EDGE('',*,*,#3895,.T.);
#5404=ORIENTED_EDGE('',*,*,#3893,.T.);
#5405=ORIENTED_EDGE('',*,*,#3895,.F.);
#5406=ORIENTED_EDGE('',*,*,#3896,.F.);
#5407=ORIENTED_EDGE('',*,*,#3897,.T.);
#5408=ORIENTED_EDGE('',*,*,#3894,.T.);
#5409=ORIENTED_EDGE('',*,*,#3897,.F.);
#5410=ORIENTED_EDGE('',*,*,#3898,.F.);
#5411=ORIENTED_EDGE('',*,*,#3899,.T.);
#5412=ORIENTED_EDGE('',*,*,#3896,.T.);
#5413=ORIENTED_EDGE('',*,*,#3899,.F.);
#5414=ORIENTED_EDGE('',*,*,#3898,.T.);
#5415=ORIENTED_EDGE('',*,*,#3900,.F.);
#5416=ORIENTED_EDGE('',*,*,#3901,.F.);
#5417=ORIENTED_EDGE('',*,*,#3902,.T.);
#5418=ORIENTED_EDGE('',*,*,#3900,.T.);
#5419=ORIENTED_EDGE('',*,*,#3902,.F.);
#5420=ORIENTED_EDGE('',*,*,#3903,.F.);
#5421=ORIENTED_EDGE('',*,*,#3904,.T.);
#5422=ORIENTED_EDGE('',*,*,#3901,.T.);
#5423=ORIENTED_EDGE('',*,*,#3904,.F.);
#5424=ORIENTED_EDGE('',*,*,#3905,.F.);
#5425=ORIENTED_EDGE('',*,*,#3906,.T.);
#5426=ORIENTED_EDGE('',*,*,#3903,.T.);
#5427=ORIENTED_EDGE('',*,*,#3906,.F.);
#5428=ORIENTED_EDGE('',*,*,#3905,.T.);
#5429=ORIENTED_EDGE('',*,*,#3907,.T.);
#5430=ORIENTED_EDGE('',*,*,#3908,.T.);
#5431=ORIENTED_EDGE('',*,*,#3909,.T.);
#5432=ORIENTED_EDGE('',*,*,#3910,.F.);
#5433=ORIENTED_EDGE('',*,*,#3911,.T.);
#5434=ORIENTED_EDGE('',*,*,#3912,.T.);
#5435=ORIENTED_EDGE('',*,*,#3913,.T.);
#5436=ORIENTED_EDGE('',*,*,#3908,.F.);
#5437=ORIENTED_EDGE('',*,*,#3914,.T.);
#5438=ORIENTED_EDGE('',*,*,#3915,.T.);
#5439=ORIENTED_EDGE('',*,*,#3916,.T.);
#5440=ORIENTED_EDGE('',*,*,#3912,.F.);
#5441=ORIENTED_EDGE('',*,*,#3917,.T.);
#5442=ORIENTED_EDGE('',*,*,#3918,.T.);
#5443=ORIENTED_EDGE('',*,*,#3919,.T.);
#5444=ORIENTED_EDGE('',*,*,#3915,.F.);
#5445=ORIENTED_EDGE('',*,*,#3920,.T.);
#5446=ORIENTED_EDGE('',*,*,#3921,.T.);
#5447=ORIENTED_EDGE('',*,*,#3922,.T.);
#5448=ORIENTED_EDGE('',*,*,#3918,.F.);
#5449=ORIENTED_EDGE('',*,*,#3923,.T.);
#5450=ORIENTED_EDGE('',*,*,#3910,.T.);
#5451=ORIENTED_EDGE('',*,*,#3924,.T.);
#5452=ORIENTED_EDGE('',*,*,#3921,.F.);
#5453=ORIENTED_EDGE('',*,*,#3923,.F.);
#5454=ORIENTED_EDGE('',*,*,#3920,.F.);
#5455=ORIENTED_EDGE('',*,*,#3917,.F.);
#5456=ORIENTED_EDGE('',*,*,#3914,.F.);
#5457=ORIENTED_EDGE('',*,*,#3911,.F.);
#5458=ORIENTED_EDGE('',*,*,#3907,.F.);
#5459=ORIENTED_EDGE('',*,*,#3924,.F.);
#5460=ORIENTED_EDGE('',*,*,#3909,.F.);
#5461=ORIENTED_EDGE('',*,*,#3913,.F.);
#5462=ORIENTED_EDGE('',*,*,#3916,.F.);
#5463=ORIENTED_EDGE('',*,*,#3919,.F.);
#5464=ORIENTED_EDGE('',*,*,#3922,.F.);
#5465=ORIENTED_EDGE('',*,*,#3925,.F.);
#5466=ORIENTED_EDGE('',*,*,#3926,.T.);
#5467=ORIENTED_EDGE('',*,*,#3927,.T.);
#5468=ORIENTED_EDGE('',*,*,#3928,.F.);
#5469=ORIENTED_EDGE('',*,*,#3929,.F.);
#5470=ORIENTED_EDGE('',*,*,#3930,.T.);
#5471=ORIENTED_EDGE('',*,*,#3931,.T.);
#5472=ORIENTED_EDGE('',*,*,#3926,.F.);
#5473=ORIENTED_EDGE('',*,*,#3932,.F.);
#5474=ORIENTED_EDGE('',*,*,#3933,.T.);
#5475=ORIENTED_EDGE('',*,*,#3934,.T.);
#5476=ORIENTED_EDGE('',*,*,#3930,.F.);
#5477=ORIENTED_EDGE('',*,*,#3935,.F.);
#5478=ORIENTED_EDGE('',*,*,#3936,.T.);
#5479=ORIENTED_EDGE('',*,*,#3937,.T.);
#5480=ORIENTED_EDGE('',*,*,#3933,.F.);
#5481=ORIENTED_EDGE('',*,*,#3938,.F.);
#5482=ORIENTED_EDGE('',*,*,#3939,.T.);
#5483=ORIENTED_EDGE('',*,*,#3940,.T.);
#5484=ORIENTED_EDGE('',*,*,#3936,.F.);
#5485=ORIENTED_EDGE('',*,*,#3941,.F.);
#5486=ORIENTED_EDGE('',*,*,#3928,.T.);
#5487=ORIENTED_EDGE('',*,*,#3942,.T.);
#5488=ORIENTED_EDGE('',*,*,#3939,.F.);
#5489=ORIENTED_EDGE('',*,*,#3942,.F.);
#5490=ORIENTED_EDGE('',*,*,#3927,.F.);
#5491=ORIENTED_EDGE('',*,*,#3931,.F.);
#5492=ORIENTED_EDGE('',*,*,#3934,.F.);
#5493=ORIENTED_EDGE('',*,*,#3937,.F.);
#5494=ORIENTED_EDGE('',*,*,#3940,.F.);
#5495=ORIENTED_EDGE('',*,*,#3943,.F.);
#5496=ORIENTED_EDGE('',*,*,#3925,.T.);
#5497=ORIENTED_EDGE('',*,*,#3941,.T.);
#5498=ORIENTED_EDGE('',*,*,#3938,.T.);
#5499=ORIENTED_EDGE('',*,*,#3935,.T.);
#5500=ORIENTED_EDGE('',*,*,#3932,.T.);
#5501=ORIENTED_EDGE('',*,*,#3929,.T.);
#5502=ORIENTED_EDGE('',*,*,#3944,.F.);
#5503=ORIENTED_EDGE('',*,*,#3945,.T.);
#5504=ORIENTED_EDGE('',*,*,#3943,.T.);
#5505=ORIENTED_EDGE('',*,*,#3945,.F.);
#5506=ORIENTED_EDGE('',*,*,#3946,.F.);
#5507=ORIENTED_EDGE('',*,*,#3947,.T.);
#5508=ORIENTED_EDGE('',*,*,#3944,.T.);
#5509=ORIENTED_EDGE('',*,*,#3947,.F.);
#5510=ORIENTED_EDGE('',*,*,#3948,.F.);
#5511=ORIENTED_EDGE('',*,*,#3949,.T.);
#5512=ORIENTED_EDGE('',*,*,#3946,.T.);
#5513=ORIENTED_EDGE('',*,*,#3949,.F.);
#5514=ORIENTED_EDGE('',*,*,#3948,.T.);
#5515=ORIENTED_EDGE('',*,*,#3950,.F.);
#5516=ORIENTED_EDGE('',*,*,#3951,.F.);
#5517=ORIENTED_EDGE('',*,*,#3952,.F.);
#5518=ORIENTED_EDGE('',*,*,#3953,.F.);
#5519=ORIENTED_EDGE('',*,*,#3954,.F.);
#5520=ORIENTED_EDGE('',*,*,#3955,.F.);
#5521=ORIENTED_EDGE('',*,*,#3956,.F.);
#5522=ORIENTED_EDGE('',*,*,#3957,.F.);
#5523=ORIENTED_EDGE('',*,*,#3954,.T.);
#5524=ORIENTED_EDGE('',*,*,#3958,.T.);
#5525=ORIENTED_EDGE('',*,*,#3959,.T.);
#5526=ORIENTED_EDGE('',*,*,#3960,.T.);
#5527=ORIENTED_EDGE('',*,*,#3953,.T.);
#5528=ORIENTED_EDGE('',*,*,#3961,.F.);
#5529=ORIENTED_EDGE('',*,*,#3962,.T.);
#5530=ORIENTED_EDGE('',*,*,#3958,.F.);
#5531=ORIENTED_EDGE('',*,*,#3952,.T.);
#5532=ORIENTED_EDGE('',*,*,#3963,.T.);
#5533=ORIENTED_EDGE('',*,*,#3964,.T.);
#5534=ORIENTED_EDGE('',*,*,#3961,.T.);
#5535=ORIENTED_EDGE('',*,*,#3951,.T.);
#5536=ORIENTED_EDGE('',*,*,#3965,.F.);
#5537=ORIENTED_EDGE('',*,*,#3966,.T.);
#5538=ORIENTED_EDGE('',*,*,#3963,.F.);
#5539=ORIENTED_EDGE('',*,*,#3967,.F.);
#5540=ORIENTED_EDGE('',*,*,#3968,.F.);
#5541=ORIENTED_EDGE('',*,*,#3959,.F.);
#5542=ORIENTED_EDGE('',*,*,#3962,.F.);
#5543=ORIENTED_EDGE('',*,*,#3964,.F.);
#5544=ORIENTED_EDGE('',*,*,#3966,.F.);
#5545=ORIENTED_EDGE('',*,*,#3969,.F.);
#5546=ORIENTED_EDGE('',*,*,#3970,.F.);
#5547=ORIENTED_EDGE('',*,*,#3955,.T.);
#5548=ORIENTED_EDGE('',*,*,#3960,.F.);
#5549=ORIENTED_EDGE('',*,*,#3968,.T.);
#5550=ORIENTED_EDGE('',*,*,#3971,.F.);
#5551=ORIENTED_EDGE('',*,*,#3950,.T.);
#5552=ORIENTED_EDGE('',*,*,#3972,.T.);
#5553=ORIENTED_EDGE('',*,*,#3969,.T.);
#5554=ORIENTED_EDGE('',*,*,#3965,.T.);
#5555=ORIENTED_EDGE('',*,*,#3956,.T.);
#5556=ORIENTED_EDGE('',*,*,#3971,.T.);
#5557=ORIENTED_EDGE('',*,*,#3967,.T.);
#5558=ORIENTED_EDGE('',*,*,#3973,.T.);
#5559=ORIENTED_EDGE('',*,*,#3957,.T.);
#5560=ORIENTED_EDGE('',*,*,#3973,.F.);
#5561=ORIENTED_EDGE('',*,*,#3970,.T.);
#5562=ORIENTED_EDGE('',*,*,#3972,.F.);
#5563=ORIENTED_EDGE('',*,*,#3974,.F.);
#5564=ORIENTED_EDGE('',*,*,#3975,.T.);
#5565=ORIENTED_EDGE('',*,*,#3976,.T.);
#5566=ORIENTED_EDGE('',*,*,#3975,.F.);
#5567=ORIENTED_EDGE('',*,*,#3977,.F.);
#5568=ORIENTED_EDGE('',*,*,#3978,.T.);
#5569=ORIENTED_EDGE('',*,*,#3979,.T.);
#5570=ORIENTED_EDGE('',*,*,#3978,.F.);
#5571=ORIENTED_EDGE('',*,*,#3977,.T.);
#5572=ORIENTED_EDGE('',*,*,#3974,.T.);
#5573=ORIENTED_EDGE('',*,*,#3979,.F.);
#5574=ORIENTED_EDGE('',*,*,#3976,.F.);
#5575=ORIENTED_EDGE('',*,*,#3980,.F.);
#5576=ORIENTED_EDGE('',*,*,#3981,.F.);
#5577=ORIENTED_EDGE('',*,*,#3982,.T.);
#5578=ORIENTED_EDGE('',*,*,#3983,.F.);
#5579=ORIENTED_EDGE('',*,*,#3982,.F.);
#5580=ORIENTED_EDGE('',*,*,#3984,.F.);
#5581=ORIENTED_EDGE('',*,*,#3985,.F.);
#5582=ORIENTED_EDGE('',*,*,#3986,.F.);
#5583=ORIENTED_EDGE('',*,*,#3987,.F.);
#5584=ORIENTED_EDGE('',*,*,#3988,.F.);
#5585=ORIENTED_EDGE('',*,*,#3989,.T.);
#5586=ORIENTED_EDGE('',*,*,#3990,.F.);
#5587=ORIENTED_EDGE('',*,*,#3991,.F.);
#5588=ORIENTED_EDGE('',*,*,#3992,.F.);
#5589=ORIENTED_EDGE('',*,*,#3993,.F.);
#5590=ORIENTED_EDGE('',*,*,#3994,.F.);
#5591=ORIENTED_EDGE('',*,*,#3995,.F.);
#5592=ORIENTED_EDGE('',*,*,#3989,.F.);
#5593=ORIENTED_EDGE('',*,*,#3985,.T.);
#5594=ORIENTED_EDGE('',*,*,#3996,.T.);
#5595=ORIENTED_EDGE('',*,*,#3994,.T.);
#5596=ORIENTED_EDGE('',*,*,#3997,.F.);
#5597=ORIENTED_EDGE('',*,*,#3984,.T.);
#5598=ORIENTED_EDGE('',*,*,#3998,.T.);
#5599=ORIENTED_EDGE('',*,*,#3995,.T.);
#5600=ORIENTED_EDGE('',*,*,#3996,.F.);
#5601=ORIENTED_EDGE('',*,*,#3981,.T.);
#5602=ORIENTED_EDGE('',*,*,#3999,.T.);
#5603=ORIENTED_EDGE('',*,*,#3990,.T.);
#5604=ORIENTED_EDGE('',*,*,#3998,.F.);
#5605=ORIENTED_EDGE('',*,*,#4000,.F.);
#5606=ORIENTED_EDGE('',*,*,#4001,.T.);
#5607=ORIENTED_EDGE('',*,*,#4002,.T.);
#5608=ORIENTED_EDGE('',*,*,#4001,.F.);
#5609=ORIENTED_EDGE('',*,*,#3980,.T.);
#5610=ORIENTED_EDGE('',*,*,#4003,.T.);
#5611=ORIENTED_EDGE('',*,*,#3991,.T.);
#5612=ORIENTED_EDGE('',*,*,#3999,.F.);
#5613=ORIENTED_EDGE('',*,*,#3986,.T.);
#5614=ORIENTED_EDGE('',*,*,#3997,.T.);
#5615=ORIENTED_EDGE('',*,*,#3993,.T.);
#5616=ORIENTED_EDGE('',*,*,#4004,.F.);
#5617=ORIENTED_EDGE('',*,*,#3987,.T.);
#5618=ORIENTED_EDGE('',*,*,#4004,.T.);
#5619=ORIENTED_EDGE('',*,*,#3992,.T.);
#5620=ORIENTED_EDGE('',*,*,#4003,.F.);
#5621=ORIENTED_EDGE('',*,*,#3988,.T.);
#5622=ORIENTED_EDGE('',*,*,#4000,.T.);
#5623=ORIENTED_EDGE('',*,*,#3983,.T.);
#5624=ORIENTED_EDGE('',*,*,#4002,.F.);
#5625=CYLINDRICAL_SURFACE('',#6462,0.25);
#5626=CYLINDRICAL_SURFACE('',#6465,0.25);
#5627=CYLINDRICAL_SURFACE('',#6475,0.33);
#5628=CYLINDRICAL_SURFACE('',#6478,0.33);
#5629=CYLINDRICAL_SURFACE('',#6481,0.44);
#5630=CYLINDRICAL_SURFACE('',#6484,0.44);
#5631=CYLINDRICAL_SURFACE('',#6487,0.44);
#5632=CYLINDRICAL_SURFACE('',#6490,0.44);
#5633=CYLINDRICAL_SURFACE('',#6493,3.1);
#5634=CYLINDRICAL_SURFACE('',#6505,0.425);
#5635=CYLINDRICAL_SURFACE('',#6508,0.595);
#5636=CYLINDRICAL_SURFACE('',#6514,0.425);
#5637=CYLINDRICAL_SURFACE('',#6517,0.595);
#5638=CYLINDRICAL_SURFACE('',#6523,0.425);
#5639=CYLINDRICAL_SURFACE('',#6526,0.595);
#5640=CYLINDRICAL_SURFACE('',#6532,0.425);
#5641=CYLINDRICAL_SURFACE('',#6535,0.595);
#5642=CYLINDRICAL_SURFACE('',#6569,0.5);
#5643=CYLINDRICAL_SURFACE('',#6577,0.2942);
#5644=CYLINDRICAL_SURFACE('',#6580,2.05);
#5645=CYLINDRICAL_SURFACE('',#6583,2.05);
#5646=CYLINDRICAL_SURFACE('',#6588,3.);
#5647=CYLINDRICAL_SURFACE('',#6591,3.);
#5648=CYLINDRICAL_SURFACE('',#6596,0.6);
#5649=CYLINDRICAL_SURFACE('',#6599,0.6);
#5650=CYLINDRICAL_SURFACE('',#6602,0.6);
#5651=CYLINDRICAL_SURFACE('',#6605,0.6);
#5652=CYLINDRICAL_SURFACE('',#6619,1.8);
#5653=CYLINDRICAL_SURFACE('',#6628,0.25);
#5654=CYLINDRICAL_SURFACE('',#6629,0.25);
#5655=CYLINDRICAL_SURFACE('',#6630,1.65);
#5656=CYLINDRICAL_SURFACE('',#6633,0.25);
#5657=CYLINDRICAL_SURFACE('',#6634,0.25);
#5658=CYLINDRICAL_SURFACE('',#6635,0.25);
#5659=CYLINDRICAL_SURFACE('',#6636,0.25);
#5660=CYLINDRICAL_SURFACE('',#6641,1.75);
#5661=CYLINDRICAL_SURFACE('',#6645,1.);
#5662=CYLINDRICAL_SURFACE('',#6653,0.65);
#5663=CYLINDRICAL_SURFACE('',#6661,0.3933);
#5664=CYLINDRICAL_SURFACE('',#6683,0.21);
#5665=CYLINDRICAL_SURFACE('',#6694,0.4);
#5666=CYLINDRICAL_SURFACE('',#6698,0.6);
#5667=CYLINDRICAL_SURFACE('',#6702,1.);
#5668=CYLINDRICAL_SURFACE('',#6708,0.605);
#5669=CYLINDRICAL_SURFACE('',#6711,0.9);
#5670=CYLINDRICAL_SURFACE('',#6717,0.605);
#5671=CYLINDRICAL_SURFACE('',#6720,0.9);
#5672=CYLINDRICAL_SURFACE('',#6726,0.275);
#5673=CYLINDRICAL_SURFACE('',#6729,1.);
#5674=CYLINDRICAL_SURFACE('',#6737,0.21);
#5675=CYLINDRICAL_SURFACE('',#6741,1.005);
#5676=CYLINDRICAL_SURFACE('',#6744,1.5);
#5677=CYLINDRICAL_SURFACE('',#6752,0.21);
#5678=CYLINDRICAL_SURFACE('',#6756,1.005);
#5679=CYLINDRICAL_SURFACE('',#6759,1.5);
#5680=CYLINDRICAL_SURFACE('',#6777,1.);
#5681=CYLINDRICAL_SURFACE('',#6779,0.33);
#5682=CYLINDRICAL_SURFACE('',#6781,0.33);
#5683=CYLINDRICAL_SURFACE('',#6783,0.33);
#5684=CYLINDRICAL_SURFACE('',#6785,0.33);
#5685=CYLINDRICAL_SURFACE('',#6787,0.33);
#5686=CYLINDRICAL_SURFACE('',#6789,0.33);
#5687=CYLINDRICAL_SURFACE('',#6794,6.);
#5688=CYLINDRICAL_SURFACE('',#6795,1.8);
#5689=CYLINDRICAL_SURFACE('',#6799,0.425);
#5690=CYLINDRICAL_SURFACE('',#6802,1.4);
#5691=CYLINDRICAL_SURFACE('',#6815,0.6);
#5692=CYLINDRICAL_SURFACE('',#6817,0.125);
#5693=CYLINDRICAL_SURFACE('',#6818,0.125);
#5694=CYLINDRICAL_SURFACE('',#6819,1.);
#5695=CYLINDRICAL_SURFACE('',#6822,0.125);
#5696=CYLINDRICAL_SURFACE('',#6823,0.125);
#5697=CYLINDRICAL_SURFACE('',#6907,1.4);
#5698=CYLINDRICAL_SURFACE('',#6992,1.4);
#5699=CYLINDRICAL_SURFACE('',#6993,0.0555000000000001);
#5700=CYLINDRICAL_SURFACE('',#6994,1.24783954473516);
#5701=CYLINDRICAL_SURFACE('',#6995,0.0555000000000001);
#5702=CYLINDRICAL_SURFACE('',#6996,1.24783954473516);
#5703=CYLINDRICAL_SURFACE('',#6997,0.0555000000000001);
#5704=CYLINDRICAL_SURFACE('',#6998,1.24783954473516);
#5705=CYLINDRICAL_SURFACE('',#6999,0.0555000000000001);
#5706=CYLINDRICAL_SURFACE('',#7000,1.24783954473516);
#5707=CYLINDRICAL_SURFACE('',#7001,0.0555000000000001);
#5708=CYLINDRICAL_SURFACE('',#7002,1.24783954473516);
#5709=CYLINDRICAL_SURFACE('',#7003,0.0555000000000001);
#5710=CYLINDRICAL_SURFACE('',#7004,1.24783954473516);
#5711=CYLINDRICAL_SURFACE('',#7005,0.0555000000000001);
#5712=CYLINDRICAL_SURFACE('',#7006,1.24783954473516);
#5713=CYLINDRICAL_SURFACE('',#7007,0.0555000000000001);
#5714=CYLINDRICAL_SURFACE('',#7008,1.24783954473516);
#5715=CYLINDRICAL_SURFACE('',#7009,0.0555000000000001);
#5716=CYLINDRICAL_SURFACE('',#7010,1.24783954473516);
#5717=CYLINDRICAL_SURFACE('',#7011,0.0555000000000001);
#5718=CYLINDRICAL_SURFACE('',#7012,1.24783954473516);
#5719=CYLINDRICAL_SURFACE('',#7013,0.0555000000000001);
#5720=CYLINDRICAL_SURFACE('',#7014,1.24783954473516);
#5721=CYLINDRICAL_SURFACE('',#7015,0.0555000000000001);
#5722=CYLINDRICAL_SURFACE('',#7016,1.24783954473516);
#5723=CYLINDRICAL_SURFACE('',#7017,0.0555000000000001);
#5724=CYLINDRICAL_SURFACE('',#7018,1.24783954473516);
#5725=CYLINDRICAL_SURFACE('',#7019,0.0555000000000001);
#5726=CYLINDRICAL_SURFACE('',#7020,1.24783954473516);
#5727=CYLINDRICAL_SURFACE('',#7021,0.0555000000000001);
#5728=CYLINDRICAL_SURFACE('',#7022,1.24783954473516);
#5729=CYLINDRICAL_SURFACE('',#7023,0.0555000000000001);
#5730=CYLINDRICAL_SURFACE('',#7024,1.24783954473516);
#5731=CYLINDRICAL_SURFACE('',#7025,0.0555000000000001);
#5732=CYLINDRICAL_SURFACE('',#7026,1.24783954473516);
#5733=CYLINDRICAL_SURFACE('',#7027,0.0555000000000001);
#5734=CYLINDRICAL_SURFACE('',#7028,1.24783954473516);
#5735=CYLINDRICAL_SURFACE('',#7029,0.0555000000000001);
#5736=CYLINDRICAL_SURFACE('',#7030,1.24783954473516);
#5737=CYLINDRICAL_SURFACE('',#7031,0.0555000000000001);
#5738=CYLINDRICAL_SURFACE('',#7032,1.24783954473516);
#5739=CYLINDRICAL_SURFACE('',#7033,0.0555000000000001);
#5740=CYLINDRICAL_SURFACE('',#7034,1.24783954473516);
#5741=CYLINDRICAL_SURFACE('',#7035,0.0555000000000001);
#5742=CYLINDRICAL_SURFACE('',#7036,1.24783954473516);
#5743=CYLINDRICAL_SURFACE('',#7037,0.0555000000000001);
#5744=CYLINDRICAL_SURFACE('',#7038,1.24783954473516);
#5745=CYLINDRICAL_SURFACE('',#7039,0.0555000000000001);
#5746=CYLINDRICAL_SURFACE('',#7040,1.24783954473516);
#5747=CYLINDRICAL_SURFACE('',#7041,0.0555000000000001);
#5748=CYLINDRICAL_SURFACE('',#7042,1.24783954473516);
#5749=CYLINDRICAL_SURFACE('',#7043,0.0555000000000001);
#5750=CYLINDRICAL_SURFACE('',#7044,1.24783954473516);
#5751=CYLINDRICAL_SURFACE('',#7045,0.0555000000000001);
#5752=CYLINDRICAL_SURFACE('',#7046,1.24783954473516);
#5753=CYLINDRICAL_SURFACE('',#7047,0.0555000000000001);
#5754=CYLINDRICAL_SURFACE('',#7048,1.24783954473516);
#5755=CYLINDRICAL_SURFACE('',#7049,0.0555000000000001);
#5756=CYLINDRICAL_SURFACE('',#7050,1.24783954473516);
#5757=CYLINDRICAL_SURFACE('',#7051,0.0555000000000001);
#5758=CYLINDRICAL_SURFACE('',#7052,1.24783954473516);
#5759=CYLINDRICAL_SURFACE('',#7053,0.0555000000000001);
#5760=CYLINDRICAL_SURFACE('',#7054,1.24783954473516);
#5761=CYLINDRICAL_SURFACE('',#7055,0.0555000000000001);
#5762=CYLINDRICAL_SURFACE('',#7056,1.24783954473516);
#5763=CYLINDRICAL_SURFACE('',#7057,0.0555000000000001);
#5764=CYLINDRICAL_SURFACE('',#7058,1.24783954473516);
#5765=CYLINDRICAL_SURFACE('',#7059,0.0555000000000001);
#5766=CYLINDRICAL_SURFACE('',#7060,1.24783954473516);
#5767=CYLINDRICAL_SURFACE('',#7061,0.0555000000000001);
#5768=CYLINDRICAL_SURFACE('',#7062,1.24783954473516);
#5769=CYLINDRICAL_SURFACE('',#7063,0.0555000000000001);
#5770=CYLINDRICAL_SURFACE('',#7064,1.24783954473516);
#5771=CYLINDRICAL_SURFACE('',#7065,0.0555000000000001);
#5772=CYLINDRICAL_SURFACE('',#7066,1.24783954473516);
#5773=CYLINDRICAL_SURFACE('',#7067,0.0555000000000001);
#5774=CYLINDRICAL_SURFACE('',#7068,1.24783954473516);
#5775=CYLINDRICAL_SURFACE('',#7069,0.0555000000000001);
#5776=CYLINDRICAL_SURFACE('',#7070,1.24783954473516);
#5777=CYLINDRICAL_SURFACE('',#7071,0.0555000000000001);
#5778=CYLINDRICAL_SURFACE('',#7072,1.24783954473516);
#5779=CYLINDRICAL_SURFACE('',#7089,0.425);
#5780=CYLINDRICAL_SURFACE('',#7097,0.24505);
#5781=CYLINDRICAL_SURFACE('',#7122,0.24505);
#5782=CYLINDRICAL_SURFACE('',#7139,0.42);
#5783=CYLINDRICAL_SURFACE('',#7142,0.8);
#5784=CYLINDRICAL_SURFACE('',#7155,0.338975);
#5785=ADVANCED_FACE('',(#674),#5625,.F.);
#5786=ADVANCED_FACE('',(#675),#5626,.F.);
#5787=ADVANCED_FACE('',(#676),#506,.T.);
#5788=ADVANCED_FACE('',(#677),#507,.T.);
#5789=ADVANCED_FACE('',(#678),#508,.T.);
#5790=ADVANCED_FACE('',(#679),#509,.T.);
#5791=ADVANCED_FACE('',(#680,#391,#392),#510,.T.);
#5792=ADVANCED_FACE('',(#681,#393,#394),#511,.F.);
#5793=ADVANCED_FACE('',(#682),#5627,.F.);
#5794=ADVANCED_FACE('',(#683),#5628,.F.);
#5795=ADVANCED_FACE('',(#684),#5629,.F.);
#5796=ADVANCED_FACE('',(#685),#5630,.F.);
#5797=ADVANCED_FACE('',(#686),#5631,.F.);
#5798=ADVANCED_FACE('',(#687),#5632,.F.);
#5799=ADVANCED_FACE('',(#688),#5633,.F.);
#5800=ADVANCED_FACE('',(#689,#395,#396),#512,.T.);
#5801=ADVANCED_FACE('',(#690),#513,.F.);
#5802=ADVANCED_FACE('',(#691,#397,#398,#399,#400,#401),#514,.T.);
#5803=ADVANCED_FACE('',(#692),#515,.T.);
#5804=ADVANCED_FACE('',(#693),#516,.T.);
#5805=ADVANCED_FACE('',(#694,#402,#403,#404,#405,#406),#517,.T.);
#5806=ADVANCED_FACE('',(#695),#518,.T.);
#5807=ADVANCED_FACE('',(#696,#407,#408),#519,.F.);
#5808=ADVANCED_FACE('',(#697),#5634,.F.);
#5809=ADVANCED_FACE('',(#698),#5635,.T.);
#5810=ADVANCED_FACE('',(#699,#409),#520,.T.);
#5811=ADVANCED_FACE('',(#700,#410),#521,.F.);
#5812=ADVANCED_FACE('',(#701),#5636,.F.);
#5813=ADVANCED_FACE('',(#702),#5637,.T.);
#5814=ADVANCED_FACE('',(#703,#411),#522,.T.);
#5815=ADVANCED_FACE('',(#704,#412),#523,.F.);
#5816=ADVANCED_FACE('',(#705),#5638,.F.);
#5817=ADVANCED_FACE('',(#706),#5639,.T.);
#5818=ADVANCED_FACE('',(#707,#413),#524,.T.);
#5819=ADVANCED_FACE('',(#708,#414),#525,.F.);
#5820=ADVANCED_FACE('',(#709),#5640,.F.);
#5821=ADVANCED_FACE('',(#710),#5641,.T.);
#5822=ADVANCED_FACE('',(#711,#415),#526,.T.);
#5823=ADVANCED_FACE('',(#712,#416),#527,.F.);
#5824=ADVANCED_FACE('',(#713),#528,.T.);
#5825=ADVANCED_FACE('',(#714),#529,.T.);
#5826=ADVANCED_FACE('',(#715),#530,.T.);
#5827=ADVANCED_FACE('',(#716),#531,.T.);
#5828=ADVANCED_FACE('',(#717),#532,.T.);
#5829=ADVANCED_FACE('',(#718),#533,.F.);
#5830=ADVANCED_FACE('',(#719),#534,.T.);
#5831=ADVANCED_FACE('',(#720),#535,.T.);
#5832=ADVANCED_FACE('',(#721),#536,.T.);
#5833=ADVANCED_FACE('',(#722),#537,.T.);
#5834=ADVANCED_FACE('',(#723),#538,.T.);
#5835=ADVANCED_FACE('',(#724),#539,.F.);
#5836=ADVANCED_FACE('',(#725),#540,.F.);
#5837=ADVANCED_FACE('',(#726),#541,.F.);
#5838=ADVANCED_FACE('',(#727),#542,.F.);
#5839=ADVANCED_FACE('',(#728),#543,.F.);
#5840=ADVANCED_FACE('',(#729),#544,.F.);
#5841=ADVANCED_FACE('',(#730),#545,.F.);
#5842=ADVANCED_FACE('',(#731),#546,.F.);
#5843=ADVANCED_FACE('',(#732),#547,.F.);
#5844=ADVANCED_FACE('',(#733),#548,.F.);
#5845=ADVANCED_FACE('',(#734),#549,.T.);
#5846=ADVANCED_FACE('',(#735),#263,.T.);
#5847=ADVANCED_FACE('',(#736),#5642,.T.);
#5848=ADVANCED_FACE('',(#737),#264,.T.);
#5849=ADVANCED_FACE('',(#738,#417),#550,.T.);
#5850=ADVANCED_FACE('',(#739),#265,.T.);
#5851=ADVANCED_FACE('',(#740),#5643,.T.);
#5852=ADVANCED_FACE('',(#741),#5644,.F.);
#5853=ADVANCED_FACE('',(#742),#5645,.F.);
#5854=ADVANCED_FACE('',(#743,#418,#419),#261,.F.);
#5855=ADVANCED_FACE('',(#744),#5646,.T.);
#5856=ADVANCED_FACE('',(#745),#5647,.T.);
#5857=ADVANCED_FACE('',(#746,#420),#551,.F.);
#5858=ADVANCED_FACE('',(#747,#421),#552,.T.);
#5859=ADVANCED_FACE('',(#748),#5648,.F.);
#5860=ADVANCED_FACE('',(#749),#5649,.F.);
#5861=ADVANCED_FACE('',(#750),#5650,.F.);
#5862=ADVANCED_FACE('',(#751),#5651,.F.);
#5863=ADVANCED_FACE('',(#752),#553,.T.);
#5864=ADVANCED_FACE('',(#753),#554,.T.);
#5865=ADVANCED_FACE('',(#754),#555,.T.);
#5866=ADVANCED_FACE('',(#755),#556,.T.);
#5867=ADVANCED_FACE('',(#756),#557,.T.);
#5868=ADVANCED_FACE('',(#757),#558,.T.);
#5869=ADVANCED_FACE('',(#758),#559,.T.);
#5870=ADVANCED_FACE('',(#759),#560,.T.);
#5871=ADVANCED_FACE('',(#760,#422,#423,#424,#425,#426),#561,.T.);
#5872=ADVANCED_FACE('',(#761,#427,#428,#429,#430,#431),#562,.F.);
#5873=ADVANCED_FACE('',(#762),#5652,.F.);
#5874=ADVANCED_FACE('',(#763,#432),#563,.T.);
#5875=ADVANCED_FACE('',(#764,#433,#434),#262,.T.);
#5876=ADVANCED_FACE('',(#765,#435),#564,.T.);
#5877=ADVANCED_FACE('',(#766),#5653,.F.);
#5878=ADVANCED_FACE('',(#767),#5654,.F.);
#5879=ADVANCED_FACE('',(#768,#436,#437,#438,#439,#440,#441),#5655,.T.);
#5880=ADVANCED_FACE('',(#769),#5656,.F.);
#5881=ADVANCED_FACE('',(#770),#5657,.F.);
#5882=ADVANCED_FACE('',(#771),#5658,.F.);
#5883=ADVANCED_FACE('',(#772),#5659,.F.);
#5884=ADVANCED_FACE('',(#773,#442),#565,.T.);
#5885=ADVANCED_FACE('',(#774,#443),#566,.T.);
#5886=ADVANCED_FACE('',(#775),#5660,.T.);
#5887=ADVANCED_FACE('',(#776,#444),#567,.T.);
#5888=ADVANCED_FACE('',(#777,#445,#446,#447,#448,#449,#450),#5661,.F.);
#5889=ADVANCED_FACE('',(#778),#568,.T.);
#5890=ADVANCED_FACE('',(#779),#266,.T.);
#5891=ADVANCED_FACE('',(#780),#5662,.T.);
#5892=ADVANCED_FACE('',(#781),#267,.T.);
#5893=ADVANCED_FACE('',(#782,#451),#569,.T.);
#5894=ADVANCED_FACE('',(#783),#268,.T.);
#5895=ADVANCED_FACE('',(#784),#5663,.T.);
#5896=ADVANCED_FACE('',(#785),#269,.T.);
#5897=ADVANCED_FACE('',(#786),#570,.T.);
#5898=ADVANCED_FACE('',(#787),#571,.F.);
#5899=ADVANCED_FACE('',(#788),#572,.F.);
#5900=ADVANCED_FACE('',(#789),#573,.F.);
#5901=ADVANCED_FACE('',(#790),#574,.F.);
#5902=ADVANCED_FACE('',(#791),#575,.F.);
#5903=ADVANCED_FACE('',(#792),#576,.F.);
#5904=ADVANCED_FACE('',(#793),#577,.F.);
#5905=ADVANCED_FACE('',(#794),#578,.F.);
#5906=ADVANCED_FACE('',(#795),#579,.F.);
#5907=ADVANCED_FACE('',(#796),#580,.T.);
#5908=ADVANCED_FACE('',(#797),#581,.F.);
#5909=ADVANCED_FACE('',(#798),#582,.F.);
#5910=ADVANCED_FACE('',(#799),#583,.F.);
#5911=ADVANCED_FACE('',(#800),#5664,.F.);
#5912=ADVANCED_FACE('',(#801),#584,.F.);
#5913=ADVANCED_FACE('',(#802),#585,.F.);
#5914=ADVANCED_FACE('',(#803),#586,.T.);
#5915=ADVANCED_FACE('',(#804),#587,.F.);
#5916=ADVANCED_FACE('',(#805),#588,.F.);
#5917=ADVANCED_FACE('',(#806),#589,.F.);
#5918=ADVANCED_FACE('',(#807),#5665,.T.);
#5919=ADVANCED_FACE('',(#808),#590,.T.);
#5920=ADVANCED_FACE('',(#809,#452),#5666,.T.);
#5921=ADVANCED_FACE('',(#810,#453),#591,.F.);
#5922=ADVANCED_FACE('',(#811,#454),#5667,.T.);
#5923=ADVANCED_FACE('',(#812,#455),#592,.T.);
#5924=ADVANCED_FACE('',(#813,#456),#593,.F.);
#5925=ADVANCED_FACE('',(#814),#5668,.F.);
#5926=ADVANCED_FACE('',(#815),#5669,.T.);
#5927=ADVANCED_FACE('',(#816,#457),#594,.T.);
#5928=ADVANCED_FACE('',(#817,#458),#595,.F.);
#5929=ADVANCED_FACE('',(#818),#5670,.F.);
#5930=ADVANCED_FACE('',(#819),#5671,.T.);
#5931=ADVANCED_FACE('',(#820,#459),#596,.T.);
#5932=ADVANCED_FACE('',(#821,#460),#597,.F.);
#5933=ADVANCED_FACE('',(#822),#5672,.F.);
#5934=ADVANCED_FACE('',(#823),#5673,.T.);
#5935=ADVANCED_FACE('',(#824,#461),#598,.T.);
#5936=ADVANCED_FACE('',(#825,#462),#599,.F.);
#5937=ADVANCED_FACE('',(#826),#600,.T.);
#5938=ADVANCED_FACE('',(#827),#5674,.F.);
#5939=ADVANCED_FACE('',(#828),#601,.T.);
#5940=ADVANCED_FACE('',(#829,#463),#5675,.F.);
#5941=ADVANCED_FACE('',(#830,#464),#5676,.T.);
#5942=ADVANCED_FACE('',(#831,#465),#602,.T.);
#5943=ADVANCED_FACE('',(#832,#466),#603,.F.);
#5944=ADVANCED_FACE('',(#833),#604,.T.);
#5945=ADVANCED_FACE('',(#834),#5677,.F.);
#5946=ADVANCED_FACE('',(#835),#605,.T.);
#5947=ADVANCED_FACE('',(#836,#467),#5678,.F.);
#5948=ADVANCED_FACE('',(#837,#468),#5679,.T.);
#5949=ADVANCED_FACE('',(#838,#469),#606,.T.);
#5950=ADVANCED_FACE('',(#839,#470),#607,.F.);
#5951=ADVANCED_FACE('',(#840),#608,.F.);
#5952=ADVANCED_FACE('',(#841),#609,.F.);
#5953=ADVANCED_FACE('',(#842),#610,.F.);
#5954=ADVANCED_FACE('',(#843,#471,#472,#473,#474,#475,#476,#477),#611,.T.);
#5955=ADVANCED_FACE('',(#844),#5680,.F.);
#5956=ADVANCED_FACE('',(#845),#5681,.F.);
#5957=ADVANCED_FACE('',(#846),#5682,.F.);
#5958=ADVANCED_FACE('',(#847),#5683,.F.);
#5959=ADVANCED_FACE('',(#848),#5684,.F.);
#5960=ADVANCED_FACE('',(#849),#5685,.F.);
#5961=ADVANCED_FACE('',(#850),#5686,.F.);
#5962=ADVANCED_FACE('',(#851,#478,#479,#480,#481,#482,#483,#484),#612,.F.);
#5963=ADVANCED_FACE('',(#852),#5687,.T.);
#5964=ADVANCED_FACE('',(#853),#5688,.T.);
#5965=ADVANCED_FACE('',(#854,#485),#613,.F.);
#5966=ADVANCED_FACE('',(#855),#5689,.F.);
#5967=ADVANCED_FACE('',(#856),#5690,.T.);
#5968=ADVANCED_FACE('',(#857,#486),#614,.T.);
#5969=ADVANCED_FACE('',(#858,#487),#615,.F.);
#5970=ADVANCED_FACE('',(#859),#616,.F.);
#5971=ADVANCED_FACE('',(#860,#488),#617,.F.);
#5972=ADVANCED_FACE('',(#861),#618,.F.);
#5973=ADVANCED_FACE('',(#862,#489),#619,.T.);
#5974=ADVANCED_FACE('',(#863,#490,#491,#492),#5691,.F.);
#5975=ADVANCED_FACE('',(#864),#5692,.F.);
#5976=ADVANCED_FACE('',(#865),#5693,.F.);
#5977=ADVANCED_FACE('',(#866,#493,#494,#495),#5694,.T.);
#5978=ADVANCED_FACE('',(#867),#5695,.F.);
#5979=ADVANCED_FACE('',(#868),#5696,.F.);
#5980=ADVANCED_FACE('',(#869,#496),#620,.F.);
#5981=ADVANCED_FACE('',(#870,#497),#621,.T.);
#5982=ADVANCED_FACE('',(#871),#5697,.T.);
#5983=ADVANCED_FACE('',(#872,#498),#622,.F.);
#5984=ADVANCED_FACE('',(#873,#499),#623,.F.);
#5985=ADVANCED_FACE('',(#874),#5698,.T.);
#5986=ADVANCED_FACE('',(#875),#5699,.F.);
#5987=ADVANCED_FACE('',(#876),#5700,.T.);
#5988=ADVANCED_FACE('',(#877),#5701,.F.);
#5989=ADVANCED_FACE('',(#878),#5702,.T.);
#5990=ADVANCED_FACE('',(#879),#5703,.F.);
#5991=ADVANCED_FACE('',(#880),#5704,.T.);
#5992=ADVANCED_FACE('',(#881),#5705,.F.);
#5993=ADVANCED_FACE('',(#882),#5706,.T.);
#5994=ADVANCED_FACE('',(#883),#5707,.F.);
#5995=ADVANCED_FACE('',(#884),#5708,.T.);
#5996=ADVANCED_FACE('',(#885),#5709,.F.);
#5997=ADVANCED_FACE('',(#886),#5710,.T.);
#5998=ADVANCED_FACE('',(#887),#5711,.F.);
#5999=ADVANCED_FACE('',(#888),#5712,.T.);
#6000=ADVANCED_FACE('',(#889),#5713,.F.);
#6001=ADVANCED_FACE('',(#890),#5714,.T.);
#6002=ADVANCED_FACE('',(#891),#5715,.F.);
#6003=ADVANCED_FACE('',(#892),#5716,.T.);
#6004=ADVANCED_FACE('',(#893),#5717,.F.);
#6005=ADVANCED_FACE('',(#894),#5718,.T.);
#6006=ADVANCED_FACE('',(#895),#5719,.F.);
#6007=ADVANCED_FACE('',(#896),#5720,.T.);
#6008=ADVANCED_FACE('',(#897),#5721,.F.);
#6009=ADVANCED_FACE('',(#898),#5722,.T.);
#6010=ADVANCED_FACE('',(#899),#5723,.F.);
#6011=ADVANCED_FACE('',(#900),#5724,.T.);
#6012=ADVANCED_FACE('',(#901),#5725,.F.);
#6013=ADVANCED_FACE('',(#902),#5726,.T.);
#6014=ADVANCED_FACE('',(#903),#5727,.F.);
#6015=ADVANCED_FACE('',(#904),#5728,.T.);
#6016=ADVANCED_FACE('',(#905),#5729,.F.);
#6017=ADVANCED_FACE('',(#906),#5730,.T.);
#6018=ADVANCED_FACE('',(#907),#5731,.F.);
#6019=ADVANCED_FACE('',(#908),#5732,.T.);
#6020=ADVANCED_FACE('',(#909),#5733,.F.);
#6021=ADVANCED_FACE('',(#910),#5734,.T.);
#6022=ADVANCED_FACE('',(#911),#5735,.F.);
#6023=ADVANCED_FACE('',(#912),#5736,.T.);
#6024=ADVANCED_FACE('',(#913),#5737,.F.);
#6025=ADVANCED_FACE('',(#914),#5738,.T.);
#6026=ADVANCED_FACE('',(#915),#5739,.F.);
#6027=ADVANCED_FACE('',(#916),#5740,.T.);
#6028=ADVANCED_FACE('',(#917),#5741,.F.);
#6029=ADVANCED_FACE('',(#918),#5742,.T.);
#6030=ADVANCED_FACE('',(#919),#5743,.F.);
#6031=ADVANCED_FACE('',(#920),#5744,.T.);
#6032=ADVANCED_FACE('',(#921),#5745,.F.);
#6033=ADVANCED_FACE('',(#922),#5746,.T.);
#6034=ADVANCED_FACE('',(#923),#5747,.F.);
#6035=ADVANCED_FACE('',(#924),#5748,.T.);
#6036=ADVANCED_FACE('',(#925),#5749,.F.);
#6037=ADVANCED_FACE('',(#926),#5750,.T.);
#6038=ADVANCED_FACE('',(#927),#5751,.F.);
#6039=ADVANCED_FACE('',(#928),#5752,.T.);
#6040=ADVANCED_FACE('',(#929),#5753,.F.);
#6041=ADVANCED_FACE('',(#930),#5754,.T.);
#6042=ADVANCED_FACE('',(#931),#5755,.F.);
#6043=ADVANCED_FACE('',(#932),#5756,.T.);
#6044=ADVANCED_FACE('',(#933),#5757,.F.);
#6045=ADVANCED_FACE('',(#934),#5758,.T.);
#6046=ADVANCED_FACE('',(#935),#5759,.F.);
#6047=ADVANCED_FACE('',(#936),#5760,.T.);
#6048=ADVANCED_FACE('',(#937),#5761,.F.);
#6049=ADVANCED_FACE('',(#938),#5762,.T.);
#6050=ADVANCED_FACE('',(#939),#5763,.F.);
#6051=ADVANCED_FACE('',(#940),#5764,.T.);
#6052=ADVANCED_FACE('',(#941),#5765,.F.);
#6053=ADVANCED_FACE('',(#942),#5766,.T.);
#6054=ADVANCED_FACE('',(#943),#5767,.F.);
#6055=ADVANCED_FACE('',(#944),#5768,.T.);
#6056=ADVANCED_FACE('',(#945),#5769,.F.);
#6057=ADVANCED_FACE('',(#946),#5770,.T.);
#6058=ADVANCED_FACE('',(#947),#5771,.F.);
#6059=ADVANCED_FACE('',(#948),#5772,.T.);
#6060=ADVANCED_FACE('',(#949),#5773,.F.);
#6061=ADVANCED_FACE('',(#950),#5774,.T.);
#6062=ADVANCED_FACE('',(#951),#5775,.F.);
#6063=ADVANCED_FACE('',(#952),#5776,.T.);
#6064=ADVANCED_FACE('',(#953),#5777,.F.);
#6065=ADVANCED_FACE('',(#954),#5778,.T.);
#6066=ADVANCED_FACE('',(#955),#624,.T.);
#6067=ADVANCED_FACE('',(#956),#625,.T.);
#6068=ADVANCED_FACE('',(#957),#626,.T.);
#6069=ADVANCED_FACE('',(#958),#627,.T.);
#6070=ADVANCED_FACE('',(#959),#628,.T.);
#6071=ADVANCED_FACE('',(#960),#629,.F.);
#6072=ADVANCED_FACE('',(#961),#630,.T.);
#6073=ADVANCED_FACE('',(#962),#631,.T.);
#6074=ADVANCED_FACE('',(#963),#632,.T.);
#6075=ADVANCED_FACE('',(#964),#633,.F.);
#6076=ADVANCED_FACE('',(#965),#634,.T.);
#6077=ADVANCED_FACE('',(#966),#270,.T.);
#6078=ADVANCED_FACE('',(#967),#5779,.T.);
#6079=ADVANCED_FACE('',(#968),#271,.T.);
#6080=ADVANCED_FACE('',(#969,#500),#635,.T.);
#6081=ADVANCED_FACE('',(#970),#272,.T.);
#6082=ADVANCED_FACE('',(#971),#5780,.T.);
#6083=ADVANCED_FACE('',(#972),#273,.T.);
#6084=ADVANCED_FACE('',(#973),#636,.T.);
#6085=ADVANCED_FACE('',(#974),#637,.F.);
#6086=ADVANCED_FACE('',(#975),#638,.F.);
#6087=ADVANCED_FACE('',(#976),#639,.F.);
#6088=ADVANCED_FACE('',(#977),#640,.F.);
#6089=ADVANCED_FACE('',(#978),#641,.F.);
#6090=ADVANCED_FACE('',(#979),#642,.F.);
#6091=ADVANCED_FACE('',(#980),#643,.F.);
#6092=ADVANCED_FACE('',(#981),#644,.F.);
#6093=ADVANCED_FACE('',(#982),#645,.F.);
#6094=ADVANCED_FACE('',(#983),#646,.F.);
#6095=ADVANCED_FACE('',(#984),#647,.F.);
#6096=ADVANCED_FACE('',(#985),#648,.F.);
#6097=ADVANCED_FACE('',(#986),#649,.F.);
#6098=ADVANCED_FACE('',(#987),#650,.F.);
#6099=ADVANCED_FACE('',(#988),#651,.F.);
#6100=ADVANCED_FACE('',(#989,#501),#652,.T.);
#6101=ADVANCED_FACE('',(#990),#274,.T.);
#6102=ADVANCED_FACE('',(#991),#5781,.T.);
#6103=ADVANCED_FACE('',(#992),#275,.T.);
#6104=ADVANCED_FACE('',(#993),#653,.T.);
#6105=ADVANCED_FACE('',(#994),#654,.F.);
#6106=ADVANCED_FACE('',(#995),#655,.T.);
#6107=ADVANCED_FACE('',(#996),#656,.T.);
#6108=ADVANCED_FACE('',(#997),#657,.T.);
#6109=ADVANCED_FACE('',(#998),#658,.T.);
#6110=ADVANCED_FACE('',(#999),#659,.T.);
#6111=ADVANCED_FACE('',(#1000),#660,.F.);
#6112=ADVANCED_FACE('',(#1001),#661,.T.);
#6113=ADVANCED_FACE('',(#1002),#662,.T.);
#6114=ADVANCED_FACE('',(#1003),#663,.T.);
#6115=ADVANCED_FACE('',(#1004),#5782,.F.);
#6116=ADVANCED_FACE('',(#1005),#5783,.T.);
#6117=ADVANCED_FACE('',(#1006,#502),#664,.T.);
#6118=ADVANCED_FACE('',(#1007,#503),#665,.F.);
#6119=ADVANCED_FACE('',(#1008),#276,.T.);
#6120=ADVANCED_FACE('',(#1009),#277,.T.);
#6121=ADVANCED_FACE('',(#1010),#666,.T.);
#6122=ADVANCED_FACE('',(#1011),#667,.T.);
#6123=ADVANCED_FACE('',(#1012),#668,.T.);
#6124=ADVANCED_FACE('',(#1013),#5784,.F.);
#6125=ADVANCED_FACE('',(#1014),#669,.T.);
#6126=ADVANCED_FACE('',(#1015),#670,.T.);
#6127=ADVANCED_FACE('',(#1016),#671,.T.);
#6128=ADVANCED_FACE('',(#1017,#504),#672,.T.);
#6129=ADVANCED_FACE('',(#1018,#505),#673,.F.);
#6130=CLOSED_SHELL('',(#5785,#5786,#5787,#5788,#5789,#5790,#5791,#5792));
#6131=CLOSED_SHELL('',(#5793,#5794,#5795,#5796,#5797,#5798,#5799,#5800,
#5801,#5802,#5803,#5804,#5805,#5806,#5807));
#6132=CLOSED_SHELL('',(#5808,#5809,#5810,#5811));
#6133=CLOSED_SHELL('',(#5812,#5813,#5814,#5815));
#6134=CLOSED_SHELL('',(#5816,#5817,#5818,#5819));
#6135=CLOSED_SHELL('',(#5820,#5821,#5822,#5823));
#6136=CLOSED_SHELL('',(#5824,#5825,#5826,#5827,#5828,#5829));
#6137=CLOSED_SHELL('',(#5830,#5831,#5832,#5833,#5834,#5835));
#6138=CLOSED_SHELL('',(#5836,#5837,#5838,#5839,#5840,#5841,#5842,#5843));
#6139=CLOSED_SHELL('',(#5844,#5845,#5846,#5847,#5848,#5849,#5850,#5851));
#6140=CLOSED_SHELL('',(#5852,#5853,#5854,#5855,#5856,#5857,#5858,#5859,
#5860,#5861,#5862,#5863,#5864,#5865,#5866,#5867,#5868,#5869,#5870,#5871,
#5872));
#6141=CLOSED_SHELL('',(#5873,#5874,#5875,#5876));
#6142=CLOSED_SHELL('',(#5877,#5878,#5879,#5880,#5881,#5882,#5883,#5884,
#5885,#5886,#5887,#5888));
#6143=CLOSED_SHELL('',(#5889,#5890,#5891,#5892,#5893,#5894,#5895,#5896,
#5897));
#6144=CLOSED_SHELL('',(#5898,#5899,#5900,#5901,#5902,#5903,#5904,#5905));
#6145=CLOSED_SHELL('',(#5906,#5907,#5908,#5909,#5910,#5911,#5912,#5913,
#5914,#5915,#5916,#5917,#5918,#5919,#5920,#5921,#5922,#5923,#5924));
#6146=CLOSED_SHELL('',(#5925,#5926,#5927,#5928));
#6147=CLOSED_SHELL('',(#5929,#5930,#5931,#5932));
#6148=CLOSED_SHELL('',(#5933,#5934,#5935,#5936));
#6149=CLOSED_SHELL('',(#5937,#5938,#5939,#5940,#5941,#5942,#5943));
#6150=CLOSED_SHELL('',(#5944,#5945,#5946,#5947,#5948,#5949,#5950));
#6151=CLOSED_SHELL('',(#5951,#5952,#5953,#5954,#5955,#5956,#5957,#5958,
#5959,#5960,#5961,#5962,#5963,#5964,#5965));
#6152=CLOSED_SHELL('',(#5966,#5967,#5968,#5969));
#6153=CLOSED_SHELL('',(#5970,#5971,#5972,#5973,#5974,#5975,#5976,#5977,
#5978,#5979,#5980,#5981,#5982,#5983,#5984,#5985,#5986,#5987,#5988,#5989,
#5990,#5991,#5992,#5993,#5994,#5995,#5996,#5997,#5998,#5999,#6000,#6001,
#6002,#6003,#6004,#6005,#6006,#6007,#6008,#6009,#6010,#6011,#6012,#6013,
#6014,#6015,#6016,#6017,#6018,#6019,#6020,#6021,#6022,#6023,#6024,#6025,
#6026,#6027,#6028,#6029,#6030,#6031,#6032,#6033,#6034,#6035,#6036,#6037,
#6038,#6039,#6040,#6041,#6042,#6043,#6044,#6045,#6046,#6047,#6048,#6049,
#6050,#6051,#6052,#6053,#6054,#6055,#6056,#6057,#6058,#6059,#6060,#6061,
#6062,#6063,#6064,#6065));
#6154=CLOSED_SHELL('',(#6066,#6067,#6068,#6069,#6070,#6071,#6072,#6073,
#6074,#6075));
#6155=CLOSED_SHELL('',(#6076,#6077,#6078,#6079,#6080,#6081,#6082,#6083,
#6084));
#6156=CLOSED_SHELL('',(#6085,#6086,#6087,#6088,#6089,#6090,#6091,#6092));
#6157=CLOSED_SHELL('',(#6093,#6094,#6095,#6096,#6097,#6098,#6099,#6100,
#6101,#6102,#6103,#6104));
#6158=CLOSED_SHELL('',(#6105,#6106,#6107,#6108,#6109,#6110,#6111,#6112,
#6113,#6114));
#6159=CLOSED_SHELL('',(#6115,#6116,#6117,#6118));
#6160=CLOSED_SHELL('',(#6119,#6120,#6121,#6122,#6123,#6124,#6125,#6126,
#6127,#6128,#6129));
#6161=DERIVED_UNIT_ELEMENT(#6215,1.);
#6162=DERIVED_UNIT_ELEMENT(#11766,-3.);
#6163=DERIVED_UNIT_ELEMENT(#6215,1.);
#6164=DERIVED_UNIT_ELEMENT(#11766,-3.);
#6165=DERIVED_UNIT_ELEMENT(#6215,1.);
#6166=DERIVED_UNIT_ELEMENT(#11766,-3.);
#6167=DERIVED_UNIT_ELEMENT(#6215,1.);
#6168=DERIVED_UNIT_ELEMENT(#11766,-3.);
#6169=DERIVED_UNIT_ELEMENT(#6215,1.);
#6170=DERIVED_UNIT_ELEMENT(#11766,-3.);
#6171=DERIVED_UNIT_ELEMENT(#6215,1.);
#6172=DERIVED_UNIT_ELEMENT(#11766,-3.);
#6173=DERIVED_UNIT_ELEMENT(#6215,1.);
#6174=DERIVED_UNIT_ELEMENT(#11766,-3.);
#6175=DERIVED_UNIT_ELEMENT(#6215,1.);
#6176=DERIVED_UNIT_ELEMENT(#11766,-3.);
#6177=DERIVED_UNIT_ELEMENT(#6215,1.);
#6178=DERIVED_UNIT_ELEMENT(#11766,-3.);
#6179=DERIVED_UNIT_ELEMENT(#6215,1.);
#6180=DERIVED_UNIT_ELEMENT(#11766,-3.);
#6181=DERIVED_UNIT_ELEMENT(#6215,1.);
#6182=DERIVED_UNIT_ELEMENT(#11766,-3.);
#6183=DERIVED_UNIT_ELEMENT(#6215,1.);
#6184=DERIVED_UNIT_ELEMENT(#11766,-3.);
#6185=DERIVED_UNIT_ELEMENT(#6215,1.);
#6186=DERIVED_UNIT_ELEMENT(#11766,-3.);
#6187=DERIVED_UNIT_ELEMENT(#6215,1.);
#6188=DERIVED_UNIT_ELEMENT(#11766,-3.);
#6189=DERIVED_UNIT_ELEMENT(#6215,1.);
#6190=DERIVED_UNIT_ELEMENT(#11766,-3.);
#6191=DERIVED_UNIT_ELEMENT(#6215,1.);
#6192=DERIVED_UNIT_ELEMENT(#11766,-3.);
#6193=DERIVED_UNIT_ELEMENT(#6215,1.);
#6194=DERIVED_UNIT_ELEMENT(#11766,-3.);
#6195=DERIVED_UNIT_ELEMENT(#6215,1.);
#6196=DERIVED_UNIT_ELEMENT(#11766,-3.);
#6197=DERIVED_UNIT_ELEMENT(#6215,1.);
#6198=DERIVED_UNIT_ELEMENT(#11766,-3.);
#6199=DERIVED_UNIT_ELEMENT(#6215,1.);
#6200=DERIVED_UNIT_ELEMENT(#11766,-3.);
#6201=DERIVED_UNIT_ELEMENT(#6215,1.);
#6202=DERIVED_UNIT_ELEMENT(#11766,-3.);
#6203=DERIVED_UNIT_ELEMENT(#6215,1.);
#6204=DERIVED_UNIT_ELEMENT(#11766,-3.);
#6205=DERIVED_UNIT_ELEMENT(#6215,1.);
#6206=DERIVED_UNIT_ELEMENT(#11766,-3.);
#6207=DERIVED_UNIT_ELEMENT(#6215,1.);
#6208=DERIVED_UNIT_ELEMENT(#11766,-3.);
#6209=DERIVED_UNIT_ELEMENT(#6215,1.);
#6210=DERIVED_UNIT_ELEMENT(#11766,-3.);
#6211=DERIVED_UNIT_ELEMENT(#6215,1.);
#6212=DERIVED_UNIT_ELEMENT(#11766,-3.);
#6213=DERIVED_UNIT_ELEMENT(#6215,1.);
#6214=DERIVED_UNIT_ELEMENT(#11766,-3.);
#6215=(
MASS_UNIT()
NAMED_UNIT(*)
SI_UNIT(.KILO.,.GRAM.)
);
#6216=DERIVED_UNIT((#6161,#6162));
#6217=DERIVED_UNIT((#6163,#6164));
#6218=DERIVED_UNIT((#6165,#6166));
#6219=DERIVED_UNIT((#6167,#6168));
#6220=DERIVED_UNIT((#6169,#6170));
#6221=DERIVED_UNIT((#6171,#6172));
#6222=DERIVED_UNIT((#6173,#6174));
#6223=DERIVED_UNIT((#6175,#6176));
#6224=DERIVED_UNIT((#6177,#6178));
#6225=DERIVED_UNIT((#6179,#6180));
#6226=DERIVED_UNIT((#6181,#6182));
#6227=DERIVED_UNIT((#6183,#6184));
#6228=DERIVED_UNIT((#6185,#6186));
#6229=DERIVED_UNIT((#6187,#6188));
#6230=DERIVED_UNIT((#6189,#6190));
#6231=DERIVED_UNIT((#6191,#6192));
#6232=DERIVED_UNIT((#6193,#6194));
#6233=DERIVED_UNIT((#6195,#6196));
#6234=DERIVED_UNIT((#6197,#6198));
#6235=DERIVED_UNIT((#6199,#6200));
#6236=DERIVED_UNIT((#6201,#6202));
#6237=DERIVED_UNIT((#6203,#6204));
#6238=DERIVED_UNIT((#6205,#6206));
#6239=DERIVED_UNIT((#6207,#6208));
#6240=DERIVED_UNIT((#6209,#6210));
#6241=DERIVED_UNIT((#6211,#6212));
#6242=DERIVED_UNIT((#6213,#6214));
#6243=MEASURE_REPRESENTATION_ITEM('density measure',
POSITIVE_RATIO_MEASURE(7850.),#6216);
#6244=MEASURE_REPRESENTATION_ITEM('density measure',
POSITIVE_RATIO_MEASURE(7850.),#6217);
#6245=MEASURE_REPRESENTATION_ITEM('density measure',
POSITIVE_RATIO_MEASURE(7850.),#6218);
#6246=MEASURE_REPRESENTATION_ITEM('density measure',
POSITIVE_RATIO_MEASURE(7850.),#6219);
#6247=MEASURE_REPRESENTATION_ITEM('density measure',
POSITIVE_RATIO_MEASURE(7850.),#6220);
#6248=MEASURE_REPRESENTATION_ITEM('density measure',
POSITIVE_RATIO_MEASURE(7850.),#6221);
#6249=MEASURE_REPRESENTATION_ITEM('density measure',
POSITIVE_RATIO_MEASURE(7850.),#6222);
#6250=MEASURE_REPRESENTATION_ITEM('density measure',
POSITIVE_RATIO_MEASURE(7850.),#6223);
#6251=MEASURE_REPRESENTATION_ITEM('density measure',
POSITIVE_RATIO_MEASURE(7850.),#6224);
#6252=MEASURE_REPRESENTATION_ITEM('density measure',
POSITIVE_RATIO_MEASURE(7850.),#6225);
#6253=MEASURE_REPRESENTATION_ITEM('density measure',
POSITIVE_RATIO_MEASURE(7850.),#6226);
#6254=MEASURE_REPRESENTATION_ITEM('density measure',
POSITIVE_RATIO_MEASURE(7850.),#6227);
#6255=MEASURE_REPRESENTATION_ITEM('density measure',
POSITIVE_RATIO_MEASURE(7850.),#6228);
#6256=MEASURE_REPRESENTATION_ITEM('density measure',
POSITIVE_RATIO_MEASURE(7850.),#6229);
#6257=MEASURE_REPRESENTATION_ITEM('density measure',
POSITIVE_RATIO_MEASURE(7850.),#6230);
#6258=MEASURE_REPRESENTATION_ITEM('density measure',
POSITIVE_RATIO_MEASURE(7850.),#6231);
#6259=MEASURE_REPRESENTATION_ITEM('density measure',
POSITIVE_RATIO_MEASURE(7850.),#6232);
#6260=MEASURE_REPRESENTATION_ITEM('density measure',
POSITIVE_RATIO_MEASURE(7850.),#6233);
#6261=MEASURE_REPRESENTATION_ITEM('density measure',
POSITIVE_RATIO_MEASURE(7850.),#6234);
#6262=MEASURE_REPRESENTATION_ITEM('density measure',
POSITIVE_RATIO_MEASURE(7850.),#6235);
#6263=MEASURE_REPRESENTATION_ITEM('density measure',
POSITIVE_RATIO_MEASURE(7850.),#6236);
#6264=MEASURE_REPRESENTATION_ITEM('density measure',
POSITIVE_RATIO_MEASURE(7850.),#6237);
#6265=MEASURE_REPRESENTATION_ITEM('density measure',
POSITIVE_RATIO_MEASURE(7850.),#6238);
#6266=MEASURE_REPRESENTATION_ITEM('density measure',
POSITIVE_RATIO_MEASURE(7850.),#6239);
#6267=MEASURE_REPRESENTATION_ITEM('density measure',
POSITIVE_RATIO_MEASURE(7850.),#6240);
#6268=MEASURE_REPRESENTATION_ITEM('density measure',
POSITIVE_RATIO_MEASURE(7850.),#6241);
#6269=MEASURE_REPRESENTATION_ITEM('density measure',
POSITIVE_RATIO_MEASURE(7850.),#6242);
#6270=PROPERTY_DEFINITION_REPRESENTATION(#6405,#6324);
#6271=PROPERTY_DEFINITION_REPRESENTATION(#6406,#6325);
#6272=PROPERTY_DEFINITION_REPRESENTATION(#6407,#6326);
#6273=PROPERTY_DEFINITION_REPRESENTATION(#6408,#6327);
#6274=PROPERTY_DEFINITION_REPRESENTATION(#6409,#6328);
#6275=PROPERTY_DEFINITION_REPRESENTATION(#6410,#6329);
#6276=PROPERTY_DEFINITION_REPRESENTATION(#6411,#6330);
#6277=PROPERTY_DEFINITION_REPRESENTATION(#6412,#6331);
#6278=PROPERTY_DEFINITION_REPRESENTATION(#6413,#6332);
#6279=PROPERTY_DEFINITION_REPRESENTATION(#6414,#6333);
#6280=PROPERTY_DEFINITION_REPRESENTATION(#6415,#6334);
#6281=PROPERTY_DEFINITION_REPRESENTATION(#6416,#6335);
#6282=PROPERTY_DEFINITION_REPRESENTATION(#6417,#6336);
#6283=PROPERTY_DEFINITION_REPRESENTATION(#6418,#6337);
#6284=PROPERTY_DEFINITION_REPRESENTATION(#6419,#6338);
#6285=PROPERTY_DEFINITION_REPRESENTATION(#6420,#6339);
#6286=PROPERTY_DEFINITION_REPRESENTATION(#6421,#6340);
#6287=PROPERTY_DEFINITION_REPRESENTATION(#6422,#6341);
#6288=PROPERTY_DEFINITION_REPRESENTATION(#6423,#6342);
#6289=PROPERTY_DEFINITION_REPRESENTATION(#6424,#6343);
#6290=PROPERTY_DEFINITION_REPRESENTATION(#6425,#6344);
#6291=PROPERTY_DEFINITION_REPRESENTATION(#6426,#6345);
#6292=PROPERTY_DEFINITION_REPRESENTATION(#6427,#6346);
#6293=PROPERTY_DEFINITION_REPRESENTATION(#6428,#6347);
#6294=PROPERTY_DEFINITION_REPRESENTATION(#6429,#6348);
#6295=PROPERTY_DEFINITION_REPRESENTATION(#6430,#6349);
#6296=PROPERTY_DEFINITION_REPRESENTATION(#6431,#6350);
#6297=PROPERTY_DEFINITION_REPRESENTATION(#6432,#6351);
#6298=PROPERTY_DEFINITION_REPRESENTATION(#6433,#6352);
#6299=PROPERTY_DEFINITION_REPRESENTATION(#6434,#6353);
#6300=PROPERTY_DEFINITION_REPRESENTATION(#6435,#6354);
#6301=PROPERTY_DEFINITION_REPRESENTATION(#6436,#6355);
#6302=PROPERTY_DEFINITION_REPRESENTATION(#6437,#6356);
#6303=PROPERTY_DEFINITION_REPRESENTATION(#6438,#6357);
#6304=PROPERTY_DEFINITION_REPRESENTATION(#6439,#6358);
#6305=PROPERTY_DEFINITION_REPRESENTATION(#6440,#6359);
#6306=PROPERTY_DEFINITION_REPRESENTATION(#6441,#6360);
#6307=PROPERTY_DEFINITION_REPRESENTATION(#6442,#6361);
#6308=PROPERTY_DEFINITION_REPRESENTATION(#6443,#6362);
#6309=PROPERTY_DEFINITION_REPRESENTATION(#6444,#6363);
#6310=PROPERTY_DEFINITION_REPRESENTATION(#6445,#6364);
#6311=PROPERTY_DEFINITION_REPRESENTATION(#6446,#6365);
#6312=PROPERTY_DEFINITION_REPRESENTATION(#6447,#6366);
#6313=PROPERTY_DEFINITION_REPRESENTATION(#6448,#6367);
#6314=PROPERTY_DEFINITION_REPRESENTATION(#6449,#6368);
#6315=PROPERTY_DEFINITION_REPRESENTATION(#6450,#6369);
#6316=PROPERTY_DEFINITION_REPRESENTATION(#6451,#6370);
#6317=PROPERTY_DEFINITION_REPRESENTATION(#6452,#6371);
#6318=PROPERTY_DEFINITION_REPRESENTATION(#6453,#6372);
#6319=PROPERTY_DEFINITION_REPRESENTATION(#6454,#6373);
#6320=PROPERTY_DEFINITION_REPRESENTATION(#6455,#6374);
#6321=PROPERTY_DEFINITION_REPRESENTATION(#6456,#6375);
#6322=PROPERTY_DEFINITION_REPRESENTATION(#6457,#6376);
#6323=PROPERTY_DEFINITION_REPRESENTATION(#6458,#6377);
#6324=REPRESENTATION('material name',(#6378),#11735);
#6325=REPRESENTATION('density',(#6243),#11735);
#6326=REPRESENTATION('material name',(#6379),#11736);
#6327=REPRESENTATION('density',(#6244),#11736);
#6328=REPRESENTATION('material name',(#6380),#11737);
#6329=REPRESENTATION('density',(#6245),#11737);
#6330=REPRESENTATION('material name',(#6381),#11738);
#6331=REPRESENTATION('density',(#6246),#11738);
#6332=REPRESENTATION('material name',(#6382),#11739);
#6333=REPRESENTATION('density',(#6247),#11739);
#6334=REPRESENTATION('material name',(#6383),#11740);
#6335=REPRESENTATION('density',(#6248),#11740);
#6336=REPRESENTATION('material name',(#6384),#11741);
#6337=REPRESENTATION('density',(#6249),#11741);
#6338=REPRESENTATION('material name',(#6385),#11742);
#6339=REPRESENTATION('density',(#6250),#11742);
#6340=REPRESENTATION('material name',(#6386),#11743);
#6341=REPRESENTATION('density',(#6251),#11743);
#6342=REPRESENTATION('material name',(#6387),#11745);
#6343=REPRESENTATION('density',(#6252),#11745);
#6344=REPRESENTATION('material name',(#6388),#11746);
#6345=REPRESENTATION('density',(#6253),#11746);
#6346=REPRESENTATION('material name',(#6389),#11747);
#6347=REPRESENTATION('density',(#6254),#11747);
#6348=REPRESENTATION('material name',(#6390),#11749);
#6349=REPRESENTATION('density',(#6255),#11749);
#6350=REPRESENTATION('material name',(#6391),#11750);
#6351=REPRESENTATION('density',(#6256),#11750);
#6352=REPRESENTATION('material name',(#6392),#11751);
#6353=REPRESENTATION('density',(#6257),#11751);
#6354=REPRESENTATION('material name',(#6393),#11752);
#6355=REPRESENTATION('density',(#6258),#11752);
#6356=REPRESENTATION('material name',(#6394),#11753);
#6357=REPRESENTATION('density',(#6259),#11753);
#6358=REPRESENTATION('material name',(#6395),#11754);
#6359=REPRESENTATION('density',(#6260),#11754);
#6360=REPRESENTATION('material name',(#6396),#11755);
#6361=REPRESENTATION('density',(#6261),#11755);
#6362=REPRESENTATION('material name',(#6397),#11756);
#6363=REPRESENTATION('density',(#6262),#11756);
#6364=REPRESENTATION('material name',(#6398),#11757);
#6365=REPRESENTATION('density',(#6263),#11757);
#6366=REPRESENTATION('material name',(#6399),#11758);
#6367=REPRESENTATION('density',(#6264),#11758);
#6368=REPRESENTATION('material name',(#6400),#11759);
#6369=REPRESENTATION('density',(#6265),#11759);
#6370=REPRESENTATION('material name',(#6401),#11760);
#6371=REPRESENTATION('density',(#6266),#11760);
#6372=REPRESENTATION('material name',(#6402),#11761);
#6373=REPRESENTATION('density',(#6267),#11761);
#6374=REPRESENTATION('material name',(#6403),#11762);
#6375=REPRESENTATION('density',(#6268),#11762);
#6376=REPRESENTATION('material name',(#6404),#11763);
#6377=REPRESENTATION('density',(#6269),#11763);
#6378=DESCRIPTIVE_REPRESENTATION_ITEM('Steel','Steel');
#6379=DESCRIPTIVE_REPRESENTATION_ITEM('Steel','Steel');
#6380=DESCRIPTIVE_REPRESENTATION_ITEM('Steel','Steel');
#6381=DESCRIPTIVE_REPRESENTATION_ITEM('Steel','Steel');
#6382=DESCRIPTIVE_REPRESENTATION_ITEM('Steel','Steel');
#6383=DESCRIPTIVE_REPRESENTATION_ITEM('Steel','Steel');
#6384=DESCRIPTIVE_REPRESENTATION_ITEM('Steel','Steel');
#6385=DESCRIPTIVE_REPRESENTATION_ITEM('Steel','Steel');
#6386=DESCRIPTIVE_REPRESENTATION_ITEM('Steel','Steel');
#6387=DESCRIPTIVE_REPRESENTATION_ITEM('Steel','Steel');
#6388=DESCRIPTIVE_REPRESENTATION_ITEM('Steel','Steel');
#6389=DESCRIPTIVE_REPRESENTATION_ITEM('Steel','Steel');
#6390=DESCRIPTIVE_REPRESENTATION_ITEM('Steel','Steel');
#6391=DESCRIPTIVE_REPRESENTATION_ITEM('Steel','Steel');
#6392=DESCRIPTIVE_REPRESENTATION_ITEM('Steel','Steel');
#6393=DESCRIPTIVE_REPRESENTATION_ITEM('Steel','Steel');
#6394=DESCRIPTIVE_REPRESENTATION_ITEM('Steel','Steel');
#6395=DESCRIPTIVE_REPRESENTATION_ITEM('Steel','Steel');
#6396=DESCRIPTIVE_REPRESENTATION_ITEM('Steel','Steel');
#6397=DESCRIPTIVE_REPRESENTATION_ITEM('Steel','Steel');
#6398=DESCRIPTIVE_REPRESENTATION_ITEM('Steel','Steel');
#6399=DESCRIPTIVE_REPRESENTATION_ITEM('Steel','Steel');
#6400=DESCRIPTIVE_REPRESENTATION_ITEM('Steel','Steel');
#6401=DESCRIPTIVE_REPRESENTATION_ITEM('Steel','Steel');
#6402=DESCRIPTIVE_REPRESENTATION_ITEM('Steel','Steel');
#6403=DESCRIPTIVE_REPRESENTATION_ITEM('Steel','Steel');
#6404=DESCRIPTIVE_REPRESENTATION_ITEM('Steel','Steel');
#6405=PROPERTY_DEFINITION('material property','material name',#11912);
#6406=PROPERTY_DEFINITION('material property','density of part',#11912);
#6407=PROPERTY_DEFINITION('material property','material name',#11913);
#6408=PROPERTY_DEFINITION('material property','density of part',#11913);
#6409=PROPERTY_DEFINITION('material property','material name',#11914);
#6410=PROPERTY_DEFINITION('material property','density of part',#11914);
#6411=PROPERTY_DEFINITION('material property','material name',#11915);
#6412=PROPERTY_DEFINITION('material property','density of part',#11915);
#6413=PROPERTY_DEFINITION('material property','material name',#11916);
#6414=PROPERTY_DEFINITION('material property','density of part',#11916);
#6415=PROPERTY_DEFINITION('material property','material name',#11917);
#6416=PROPERTY_DEFINITION('material property','density of part',#11917);
#6417=PROPERTY_DEFINITION('material property','material name',#11918);
#6418=PROPERTY_DEFINITION('material property','density of part',#11918);
#6419=PROPERTY_DEFINITION('material property','material name',#11919);
#6420=PROPERTY_DEFINITION('material property','density of part',#11919);
#6421=PROPERTY_DEFINITION('material property','material name',#11920);
#6422=PROPERTY_DEFINITION('material property','density of part',#11920);
#6423=PROPERTY_DEFINITION('material property','material name',#11922);
#6424=PROPERTY_DEFINITION('material property','density of part',#11922);
#6425=PROPERTY_DEFINITION('material property','material name',#11923);
#6426=PROPERTY_DEFINITION('material property','density of part',#11923);
#6427=PROPERTY_DEFINITION('material property','material name',#11924);
#6428=PROPERTY_DEFINITION('material property','density of part',#11924);
#6429=PROPERTY_DEFINITION('material property','material name',#11926);
#6430=PROPERTY_DEFINITION('material property','density of part',#11926);
#6431=PROPERTY_DEFINITION('material property','material name',#11927);
#6432=PROPERTY_DEFINITION('material property','density of part',#11927);
#6433=PROPERTY_DEFINITION('material property','material name',#11928);
#6434=PROPERTY_DEFINITION('material property','density of part',#11928);
#6435=PROPERTY_DEFINITION('material property','material name',#11929);
#6436=PROPERTY_DEFINITION('material property','density of part',#11929);
#6437=PROPERTY_DEFINITION('material property','material name',#11930);
#6438=PROPERTY_DEFINITION('material property','density of part',#11930);
#6439=PROPERTY_DEFINITION('material property','material name',#11931);
#6440=PROPERTY_DEFINITION('material property','density of part',#11931);
#6441=PROPERTY_DEFINITION('material property','material name',#11932);
#6442=PROPERTY_DEFINITION('material property','density of part',#11932);
#6443=PROPERTY_DEFINITION('material property','material name',#11933);
#6444=PROPERTY_DEFINITION('material property','density of part',#11933);
#6445=PROPERTY_DEFINITION('material property','material name',#11934);
#6446=PROPERTY_DEFINITION('material property','density of part',#11934);
#6447=PROPERTY_DEFINITION('material property','material name',#11935);
#6448=PROPERTY_DEFINITION('material property','density of part',#11935);
#6449=PROPERTY_DEFINITION('material property','material name',#11936);
#6450=PROPERTY_DEFINITION('material property','density of part',#11936);
#6451=PROPERTY_DEFINITION('material property','material name',#11937);
#6452=PROPERTY_DEFINITION('material property','density of part',#11937);
#6453=PROPERTY_DEFINITION('material property','material name',#11938);
#6454=PROPERTY_DEFINITION('material property','density of part',#11938);
#6455=PROPERTY_DEFINITION('material property','material name',#11939);
#6456=PROPERTY_DEFINITION('material property','density of part',#11939);
#6457=PROPERTY_DEFINITION('material property','material name',#11940);
#6458=PROPERTY_DEFINITION('material property','density of part',#11940);
#6459=AXIS2_PLACEMENT_3D('',#9128,#7208,#7209);
#6460=AXIS2_PLACEMENT_3D('',#9129,#7210,#7211);
#6461=AXIS2_PLACEMENT_3D('',#9130,#7212,#7213);
#6462=AXIS2_PLACEMENT_3D('',#9131,#7214,#7215);
#6463=AXIS2_PLACEMENT_3D('',#9133,#7216,#7217);
#6464=AXIS2_PLACEMENT_3D('',#9136,#7219,#7220);
#6465=AXIS2_PLACEMENT_3D('',#9137,#7221,#7222);
#6466=AXIS2_PLACEMENT_3D('',#9139,#7223,#7224);
#6467=AXIS2_PLACEMENT_3D('',#9142,#7226,#7227);
#6468=AXIS2_PLACEMENT_3D('',#9143,#7228,#7229);
#6469=AXIS2_PLACEMENT_3D('',#9152,#7234,#7235);
#6470=AXIS2_PLACEMENT_3D('',#9158,#7239,#7240);
#6471=AXIS2_PLACEMENT_3D('',#9164,#7244,#7245);
#6472=AXIS2_PLACEMENT_3D('',#9167,#7248,#7249);
#6473=AXIS2_PLACEMENT_3D('',#9168,#7250,#7251);
#6474=AXIS2_PLACEMENT_3D('',#9169,#7252,#7253);
#6475=AXIS2_PLACEMENT_3D('',#9170,#7254,#7255);
#6476=AXIS2_PLACEMENT_3D('',#9172,#7256,#7257);
#6477=AXIS2_PLACEMENT_3D('',#9175,#7259,#7260);
#6478=AXIS2_PLACEMENT_3D('',#9176,#7261,#7262);
#6479=AXIS2_PLACEMENT_3D('',#9178,#7263,#7264);
#6480=AXIS2_PLACEMENT_3D('',#9181,#7266,#7267);
#6481=AXIS2_PLACEMENT_3D('',#9182,#7268,#7269);
#6482=AXIS2_PLACEMENT_3D('',#9184,#7270,#7271);
#6483=AXIS2_PLACEMENT_3D('',#9187,#7273,#7274);
#6484=AXIS2_PLACEMENT_3D('',#9188,#7275,#7276);
#6485=AXIS2_PLACEMENT_3D('',#9190,#7277,#7278);
#6486=AXIS2_PLACEMENT_3D('',#9193,#7280,#7281);
#6487=AXIS2_PLACEMENT_3D('',#9194,#7282,#7283);
#6488=AXIS2_PLACEMENT_3D('',#9196,#7284,#7285);
#6489=AXIS2_PLACEMENT_3D('',#9199,#7287,#7288);
#6490=AXIS2_PLACEMENT_3D('',#9200,#7289,#7290);
#6491=AXIS2_PLACEMENT_3D('',#9202,#7291,#7292);
#6492=AXIS2_PLACEMENT_3D('',#9205,#7294,#7295);
#6493=AXIS2_PLACEMENT_3D('',#9206,#7296,#7297);
#6494=AXIS2_PLACEMENT_3D('',#9208,#7298,#7299);
#6495=AXIS2_PLACEMENT_3D('',#9211,#7301,#7302);
#6496=AXIS2_PLACEMENT_3D('',#9212,#7303,#7304);
#6497=AXIS2_PLACEMENT_3D('',#9221,#7309,#7310);
#6498=AXIS2_PLACEMENT_3D('',#9227,#7314,#7315);
#6499=AXIS2_PLACEMENT_3D('',#9236,#7320,#7321);
#6500=AXIS2_PLACEMENT_3D('',#9241,#7325,#7326);
#6501=AXIS2_PLACEMENT_3D('',#9246,#7330,#7331);
#6502=AXIS2_PLACEMENT_3D('',#9248,#7333,#7334);
#6503=AXIS2_PLACEMENT_3D('',#9249,#7335,#7336);
#6504=AXIS2_PLACEMENT_3D('',#9250,#7337,#7338);
#6505=AXIS2_PLACEMENT_3D('',#9251,#7339,#7340);
#6506=AXIS2_PLACEMENT_3D('',#9253,#7341,#7342);
#6507=AXIS2_PLACEMENT_3D('',#9256,#7344,#7345);
#6508=AXIS2_PLACEMENT_3D('',#9257,#7346,#7347);
#6509=AXIS2_PLACEMENT_3D('',#9259,#7348,#7349);
#6510=AXIS2_PLACEMENT_3D('',#9262,#7351,#7352);
#6511=AXIS2_PLACEMENT_3D('',#9263,#7353,#7354);
#6512=AXIS2_PLACEMENT_3D('',#9264,#7355,#7356);
#6513=AXIS2_PLACEMENT_3D('',#9265,#7357,#7358);
#6514=AXIS2_PLACEMENT_3D('',#9266,#7359,#7360);
#6515=AXIS2_PLACEMENT_3D('',#9268,#7361,#7362);
#6516=AXIS2_PLACEMENT_3D('',#9271,#7364,#7365);
#6517=AXIS2_PLACEMENT_3D('',#9272,#7366,#7367);
#6518=AXIS2_PLACEMENT_3D('',#9274,#7368,#7369);
#6519=AXIS2_PLACEMENT_3D('',#9277,#7371,#7372);
#6520=AXIS2_PLACEMENT_3D('',#9278,#7373,#7374);
#6521=AXIS2_PLACEMENT_3D('',#9279,#7375,#7376);
#6522=AXIS2_PLACEMENT_3D('',#9280,#7377,#7378);
#6523=AXIS2_PLACEMENT_3D('',#9281,#7379,#7380);
#6524=AXIS2_PLACEMENT_3D('',#9283,#7381,#7382);
#6525=AXIS2_PLACEMENT_3D('',#9286,#7384,#7385);
#6526=AXIS2_PLACEMENT_3D('',#9287,#7386,#7387);
#6527=AXIS2_PLACEMENT_3D('',#9289,#7388,#7389);
#6528=AXIS2_PLACEMENT_3D('',#9292,#7391,#7392);
#6529=AXIS2_PLACEMENT_3D('',#9293,#7393,#7394);
#6530=AXIS2_PLACEMENT_3D('',#9294,#7395,#7396);
#6531=AXIS2_PLACEMENT_3D('',#9295,#7397,#7398);
#6532=AXIS2_PLACEMENT_3D('',#9296,#7399,#7400);
#6533=AXIS2_PLACEMENT_3D('',#9298,#7401,#7402);
#6534=AXIS2_PLACEMENT_3D('',#9301,#7404,#7405);
#6535=AXIS2_PLACEMENT_3D('',#9302,#7406,#7407);
#6536=AXIS2_PLACEMENT_3D('',#9304,#7408,#7409);
#6537=AXIS2_PLACEMENT_3D('',#9307,#7411,#7412);
#6538=AXIS2_PLACEMENT_3D('',#9308,#7413,#7414);
#6539=AXIS2_PLACEMENT_3D('',#9309,#7415,#7416);
#6540=AXIS2_PLACEMENT_3D('',#9310,#7417,#7418);
#6541=AXIS2_PLACEMENT_3D('',#9311,#7419,#7420);
#6542=AXIS2_PLACEMENT_3D('',#9320,#7425,#7426);
#6543=AXIS2_PLACEMENT_3D('',#9326,#7430,#7431);
#6544=AXIS2_PLACEMENT_3D('',#9332,#7435,#7436);
#6545=AXIS2_PLACEMENT_3D('',#9335,#7439,#7440);
#6546=AXIS2_PLACEMENT_3D('',#9336,#7441,#7442);
#6547=AXIS2_PLACEMENT_3D('',#9337,#7443,#7444);
#6548=AXIS2_PLACEMENT_3D('',#9338,#7445,#7446);
#6549=AXIS2_PLACEMENT_3D('',#9347,#7451,#7452);
#6550=AXIS2_PLACEMENT_3D('',#9353,#7456,#7457);
#6551=AXIS2_PLACEMENT_3D('',#9359,#7461,#7462);
#6552=AXIS2_PLACEMENT_3D('',#9362,#7465,#7466);
#6553=AXIS2_PLACEMENT_3D('',#9363,#7467,#7468);
#6554=AXIS2_PLACEMENT_3D('',#9364,#7469,#7470);
#6555=AXIS2_PLACEMENT_3D('',#9365,#7471,#7472);
#6556=AXIS2_PLACEMENT_3D('',#9374,#7477,#7478);
#6557=AXIS2_PLACEMENT_3D('',#9380,#7482,#7483);
#6558=AXIS2_PLACEMENT_3D('',#9386,#7487,#7488);
#6559=AXIS2_PLACEMENT_3D('',#9392,#7492,#7493);
#6560=AXIS2_PLACEMENT_3D('',#9398,#7497,#7498);
#6561=AXIS2_PLACEMENT_3D('',#9401,#7501,#7502);
#6562=AXIS2_PLACEMENT_3D('',#9402,#7503,#7504);
#6563=AXIS2_PLACEMENT_3D('',#9403,#7505,#7506);
#6564=AXIS2_PLACEMENT_3D('',#9405,#7507,#7508);
#6565=AXIS2_PLACEMENT_3D('',#9406,#7509,#7510);
#6566=AXIS2_PLACEMENT_3D('',#9408,#7511,#7512);
#6567=AXIS2_PLACEMENT_3D('',#9409,#7513,#7514);
#6568=AXIS2_PLACEMENT_3D('',#9411,#7515,#7516);
#6569=AXIS2_PLACEMENT_3D('',#9413,#7518,#7519);
#6570=AXIS2_PLACEMENT_3D('',#9415,#7520,#7521);
#6571=AXIS2_PLACEMENT_3D('',#9417,#7523,#7524);
#6572=AXIS2_PLACEMENT_3D('',#9419,#7525,#7526);
#6573=AXIS2_PLACEMENT_3D('',#9421,#7528,#7529);
#6574=AXIS2_PLACEMENT_3D('',#9423,#7530,#7531);
#6575=AXIS2_PLACEMENT_3D('',#9424,#7532,#7533);
#6576=AXIS2_PLACEMENT_3D('',#9426,#7534,#7535);
#6577=AXIS2_PLACEMENT_3D('',#9428,#7537,#7538);
#6578=AXIS2_PLACEMENT_3D('',#9430,#7540,#7541);
#6579=AXIS2_PLACEMENT_3D('',#9431,#7542,#7543);
#6580=AXIS2_PLACEMENT_3D('',#9432,#7544,#7545);
#6581=AXIS2_PLACEMENT_3D('',#9434,#7546,#7547);
#6582=AXIS2_PLACEMENT_3D('',#9437,#7549,#7550);
#6583=AXIS2_PLACEMENT_3D('',#9438,#7551,#7552);
#6584=AXIS2_PLACEMENT_3D('',#9440,#7553,#7554);
#6585=AXIS2_PLACEMENT_3D('',#9443,#7556,#7557);
#6586=AXIS2_PLACEMENT_3D('',#9444,#7558,#7559);
#6587=AXIS2_PLACEMENT_3D('',#9447,#7560,#7561);
#6588=AXIS2_PLACEMENT_3D('',#9448,#7562,#7563);
#6589=AXIS2_PLACEMENT_3D('',#9450,#7564,#7565);
#6590=AXIS2_PLACEMENT_3D('',#9453,#7567,#7568);
#6591=AXIS2_PLACEMENT_3D('',#9454,#7569,#7570);
#6592=AXIS2_PLACEMENT_3D('',#9456,#7571,#7572);
#6593=AXIS2_PLACEMENT_3D('',#9459,#7574,#7575);
#6594=AXIS2_PLACEMENT_3D('',#9460,#7576,#7577);
#6595=AXIS2_PLACEMENT_3D('',#9461,#7578,#7579);
#6596=AXIS2_PLACEMENT_3D('',#9462,#7580,#7581);
#6597=AXIS2_PLACEMENT_3D('',#9464,#7582,#7583);
#6598=AXIS2_PLACEMENT_3D('',#9467,#7585,#7586);
#6599=AXIS2_PLACEMENT_3D('',#9468,#7587,#7588);
#6600=AXIS2_PLACEMENT_3D('',#9470,#7589,#7590);
#6601=AXIS2_PLACEMENT_3D('',#9473,#7592,#7593);
#6602=AXIS2_PLACEMENT_3D('',#9474,#7594,#7595);
#6603=AXIS2_PLACEMENT_3D('',#9476,#7596,#7597);
#6604=AXIS2_PLACEMENT_3D('',#9479,#7599,#7600);
#6605=AXIS2_PLACEMENT_3D('',#9480,#7601,#7602);
#6606=AXIS2_PLACEMENT_3D('',#9482,#7603,#7604);
#6607=AXIS2_PLACEMENT_3D('',#9485,#7606,#7607);
#6608=AXIS2_PLACEMENT_3D('',#9486,#7608,#7609);
#6609=AXIS2_PLACEMENT_3D('',#9495,#7614,#7615);
#6610=AXIS2_PLACEMENT_3D('',#9501,#7619,#7620);
#6611=AXIS2_PLACEMENT_3D('',#9507,#7624,#7625);
#6612=AXIS2_PLACEMENT_3D('',#9513,#7629,#7630);
#6613=AXIS2_PLACEMENT_3D('',#9519,#7634,#7635);
#6614=AXIS2_PLACEMENT_3D('',#9525,#7639,#7640);
#6615=AXIS2_PLACEMENT_3D('',#9531,#7644,#7645);
#6616=AXIS2_PLACEMENT_3D('',#9534,#7648,#7649);
#6617=AXIS2_PLACEMENT_3D('',#9535,#7650,#7651);
#6618=AXIS2_PLACEMENT_3D('',#9536,#7652,#7653);
#6619=AXIS2_PLACEMENT_3D('',#9537,#7654,#7655);
#6620=AXIS2_PLACEMENT_3D('',#9539,#7656,#7657);
#6621=AXIS2_PLACEMENT_3D('',#9542,#7659,#7660);
#6622=AXIS2_PLACEMENT_3D('',#9543,#7661,#7662);
#6623=AXIS2_PLACEMENT_3D('',#9545,#7663,#7664);
#6624=AXIS2_PLACEMENT_3D('',#9546,#7665,#7666);
#6625=AXIS2_PLACEMENT_3D('',#9549,#7667,#7668);
#6626=AXIS2_PLACEMENT_3D('',#9551,#7669,#7670);
#6627=AXIS2_PLACEMENT_3D('',#9552,#7671,#7672);
#6628=AXIS2_PLACEMENT_3D('',#9553,#7673,#7674);
#6629=AXIS2_PLACEMENT_3D('',#9631,#7676,#7677);
#6630=AXIS2_PLACEMENT_3D('',#9709,#7679,#7680);
#6631=AXIS2_PLACEMENT_3D('',#9711,#7681,#7682);
#6632=AXIS2_PLACEMENT_3D('',#9714,#7684,#7685);
#6633=AXIS2_PLACEMENT_3D('',#9879,#7686,#7687);
#6634=AXIS2_PLACEMENT_3D('',#9916,#7689,#7690);
#6635=AXIS2_PLACEMENT_3D('',#9953,#7692,#7693);
#6636=AXIS2_PLACEMENT_3D('',#9990,#7695,#7696);
#6637=AXIS2_PLACEMENT_3D('',#10027,#7698,#7699);
#6638=AXIS2_PLACEMENT_3D('',#10029,#7700,#7701);
#6639=AXIS2_PLACEMENT_3D('',#10030,#7702,#7703);
#6640=AXIS2_PLACEMENT_3D('',#10032,#7704,#7705);
#6641=AXIS2_PLACEMENT_3D('',#10033,#7706,#7707);
#6642=AXIS2_PLACEMENT_3D('',#10035,#7708,#7709);
#6643=AXIS2_PLACEMENT_3D('',#10037,#7711,#7712);
#6644=AXIS2_PLACEMENT_3D('',#10039,#7713,#7714);
#6645=AXIS2_PLACEMENT_3D('',#10040,#7715,#7716);
#6646=AXIS2_PLACEMENT_3D('',#10042,#7718,#7719);
#6647=AXIS2_PLACEMENT_3D('',#10043,#7720,#7721);
#6648=AXIS2_PLACEMENT_3D('',#10044,#7722,#7723);
#6649=AXIS2_PLACEMENT_3D('',#10045,#7724,#7725);
#6650=AXIS2_PLACEMENT_3D('',#10047,#7726,#7727);
#6651=AXIS2_PLACEMENT_3D('',#10048,#7728,#7729);
#6652=AXIS2_PLACEMENT_3D('',#10050,#7730,#7731);
#6653=AXIS2_PLACEMENT_3D('',#10052,#7733,#7734);
#6654=AXIS2_PLACEMENT_3D('',#10054,#7735,#7736);
#6655=AXIS2_PLACEMENT_3D('',#10056,#7738,#7739);
#6656=AXIS2_PLACEMENT_3D('',#10058,#7740,#7741);
#6657=AXIS2_PLACEMENT_3D('',#10060,#7743,#7744);
#6658=AXIS2_PLACEMENT_3D('',#10062,#7745,#7746);
#6659=AXIS2_PLACEMENT_3D('',#10063,#7747,#7748);
#6660=AXIS2_PLACEMENT_3D('',#10065,#7749,#7750);
#6661=AXIS2_PLACEMENT_3D('',#10067,#7752,#7753);
#6662=AXIS2_PLACEMENT_3D('',#10069,#7754,#7755);
#6663=AXIS2_PLACEMENT_3D('',#10071,#7757,#7758);
#6664=AXIS2_PLACEMENT_3D('',#10073,#7759,#7760);
#6665=AXIS2_PLACEMENT_3D('',#10075,#7762,#7763);
#6666=AXIS2_PLACEMENT_3D('',#10076,#7764,#7765);
#6667=AXIS2_PLACEMENT_3D('',#10085,#7770,#7771);
#6668=AXIS2_PLACEMENT_3D('',#10091,#7775,#7776);
#6669=AXIS2_PLACEMENT_3D('',#10097,#7780,#7781);
#6670=AXIS2_PLACEMENT_3D('',#10103,#7785,#7786);
#6671=AXIS2_PLACEMENT_3D('',#10109,#7790,#7791);
#6672=AXIS2_PLACEMENT_3D('',#10112,#7794,#7795);
#6673=AXIS2_PLACEMENT_3D('',#10113,#7796,#7797);
#6674=AXIS2_PLACEMENT_3D('',#10114,#7798,#7799);
#6675=AXIS2_PLACEMENT_3D('',#10115,#7800,#7801);
#6676=AXIS2_PLACEMENT_3D('',#10116,#7802,#7803);
#6677=AXIS2_PLACEMENT_3D('',#10125,#7808,#7809);
#6678=AXIS2_PLACEMENT_3D('',#10127,#7810,#7811);
#6679=AXIS2_PLACEMENT_3D('',#10131,#7814,#7815);
#6680=AXIS2_PLACEMENT_3D('',#10137,#7819,#7820);
#6681=AXIS2_PLACEMENT_3D('',#10139,#7822,#7823);
#6682=AXIS2_PLACEMENT_3D('',#10140,#7824,#7825);
#6683=AXIS2_PLACEMENT_3D('',#10141,#7826,#7827);
#6684=AXIS2_PLACEMENT_3D('',#10143,#7828,#7829);
#6685=AXIS2_PLACEMENT_3D('',#10146,#7831,#7832);
#6686=AXIS2_PLACEMENT_3D('',#10147,#7833,#7834);
#6687=AXIS2_PLACEMENT_3D('',#10148,#7835,#7836);
#6688=AXIS2_PLACEMENT_3D('',#10157,#7841,#7842);
#6689=AXIS2_PLACEMENT_3D('',#10159,#7843,#7844);
#6690=AXIS2_PLACEMENT_3D('',#10163,#7847,#7848);
#6691=AXIS2_PLACEMENT_3D('',#10169,#7852,#7853);
#6692=AXIS2_PLACEMENT_3D('',#10171,#7855,#7856);
#6693=AXIS2_PLACEMENT_3D('',#10172,#7857,#7858);
#6694=AXIS2_PLACEMENT_3D('',#10173,#7859,#7860);
#6695=AXIS2_PLACEMENT_3D('',#10175,#7861,#7862);
#6696=AXIS2_PLACEMENT_3D('',#10178,#7864,#7865);
#6697=AXIS2_PLACEMENT_3D('',#10179,#7866,#7867);
#6698=AXIS2_PLACEMENT_3D('',#10180,#7868,#7869);
#6699=AXIS2_PLACEMENT_3D('',#10182,#7870,#7871);
#6700=AXIS2_PLACEMENT_3D('',#10185,#7873,#7874);
#6701=AXIS2_PLACEMENT_3D('',#10186,#7875,#7876);
#6702=AXIS2_PLACEMENT_3D('',#10187,#7877,#7878);
#6703=AXIS2_PLACEMENT_3D('',#10189,#7879,#7880);
#6704=AXIS2_PLACEMENT_3D('',#10192,#7882,#7883);
#6705=AXIS2_PLACEMENT_3D('',#10193,#7884,#7885);
#6706=AXIS2_PLACEMENT_3D('',#10194,#7886,#7887);
#6707=AXIS2_PLACEMENT_3D('',#10195,#7888,#7889);
#6708=AXIS2_PLACEMENT_3D('',#10196,#7890,#7891);
#6709=AXIS2_PLACEMENT_3D('',#10198,#7892,#7893);
#6710=AXIS2_PLACEMENT_3D('',#10201,#7895,#7896);
#6711=AXIS2_PLACEMENT_3D('',#10202,#7897,#7898);
#6712=AXIS2_PLACEMENT_3D('',#10204,#7899,#7900);
#6713=AXIS2_PLACEMENT_3D('',#10207,#7902,#7903);
#6714=AXIS2_PLACEMENT_3D('',#10208,#7904,#7905);
#6715=AXIS2_PLACEMENT_3D('',#10209,#7906,#7907);
#6716=AXIS2_PLACEMENT_3D('',#10210,#7908,#7909);
#6717=AXIS2_PLACEMENT_3D('',#10211,#7910,#7911);
#6718=AXIS2_PLACEMENT_3D('',#10213,#7912,#7913);
#6719=AXIS2_PLACEMENT_3D('',#10216,#7915,#7916);
#6720=AXIS2_PLACEMENT_3D('',#10217,#7917,#7918);
#6721=AXIS2_PLACEMENT_3D('',#10219,#7919,#7920);
#6722=AXIS2_PLACEMENT_3D('',#10222,#7922,#7923);
#6723=AXIS2_PLACEMENT_3D('',#10223,#7924,#7925);
#6724=AXIS2_PLACEMENT_3D('',#10224,#7926,#7927);
#6725=AXIS2_PLACEMENT_3D('',#10225,#7928,#7929);
#6726=AXIS2_PLACEMENT_3D('',#10226,#7930,#7931);
#6727=AXIS2_PLACEMENT_3D('',#10228,#7932,#7933);
#6728=AXIS2_PLACEMENT_3D('',#10231,#7935,#7936);
#6729=AXIS2_PLACEMENT_3D('',#10232,#7937,#7938);
#6730=AXIS2_PLACEMENT_3D('',#10234,#7939,#7940);
#6731=AXIS2_PLACEMENT_3D('',#10237,#7942,#7943);
#6732=AXIS2_PLACEMENT_3D('',#10238,#7944,#7945);
#6733=AXIS2_PLACEMENT_3D('',#10239,#7946,#7947);
#6734=AXIS2_PLACEMENT_3D('',#10240,#7948,#7949);
#6735=AXIS2_PLACEMENT_3D('',#10241,#7950,#7951);
#6736=AXIS2_PLACEMENT_3D('',#10245,#7953,#7954);
#6737=AXIS2_PLACEMENT_3D('',#10246,#7955,#7956);
#6738=AXIS2_PLACEMENT_3D('',#10263,#7957,#7958);
#6739=AXIS2_PLACEMENT_3D('',#10304,#7960,#7961);
#6740=AXIS2_PLACEMENT_3D('',#10319,#7962,#7963);
#6741=AXIS2_PLACEMENT_3D('',#10321,#7965,#7966);
#6742=AXIS2_PLACEMENT_3D('',#10323,#7967,#7968);
#6743=AXIS2_PLACEMENT_3D('',#10326,#7970,#7971);
#6744=AXIS2_PLACEMENT_3D('',#10327,#7972,#7973);
#6745=AXIS2_PLACEMENT_3D('',#10329,#7974,#7975);
#6746=AXIS2_PLACEMENT_3D('',#10332,#7977,#7978);
#6747=AXIS2_PLACEMENT_3D('',#10333,#7979,#7980);
#6748=AXIS2_PLACEMENT_3D('',#10334,#7981,#7982);
#6749=AXIS2_PLACEMENT_3D('',#10335,#7983,#7984);
#6750=AXIS2_PLACEMENT_3D('',#10336,#7985,#7986);
#6751=AXIS2_PLACEMENT_3D('',#10340,#7988,#7989);
#6752=AXIS2_PLACEMENT_3D('',#10341,#7990,#7991);
#6753=AXIS2_PLACEMENT_3D('',#10358,#7992,#7993);
#6754=AXIS2_PLACEMENT_3D('',#10399,#7995,#7996);
#6755=AXIS2_PLACEMENT_3D('',#10414,#7997,#7998);
#6756=AXIS2_PLACEMENT_3D('',#10416,#8000,#8001);
#6757=AXIS2_PLACEMENT_3D('',#10418,#8002,#8003);
#6758=AXIS2_PLACEMENT_3D('',#10421,#8005,#8006);
#6759=AXIS2_PLACEMENT_3D('',#10422,#8007,#8008);
#6760=AXIS2_PLACEMENT_3D('',#10424,#8009,#8010);
#6761=AXIS2_PLACEMENT_3D('',#10427,#8012,#8013);
#6762=AXIS2_PLACEMENT_3D('',#10428,#8014,#8015);
#6763=AXIS2_PLACEMENT_3D('',#10429,#8016,#8017);
#6764=AXIS2_PLACEMENT_3D('',#10430,#8018,#8019);
#6765=AXIS2_PLACEMENT_3D('',#10431,#8020,#8021);
#6766=AXIS2_PLACEMENT_3D('',#10440,#8026,#8027);
#6767=AXIS2_PLACEMENT_3D('',#10446,#8031,#8032);
#6768=AXIS2_PLACEMENT_3D('',#10452,#8036,#8037);
#6769=AXIS2_PLACEMENT_3D('',#10454,#8038,#8039);
#6770=AXIS2_PLACEMENT_3D('',#10456,#8040,#8041);
#6771=AXIS2_PLACEMENT_3D('',#10458,#8042,#8043);
#6772=AXIS2_PLACEMENT_3D('',#10460,#8044,#8045);
#6773=AXIS2_PLACEMENT_3D('',#10462,#8046,#8047);
#6774=AXIS2_PLACEMENT_3D('',#10464,#8048,#8049);
#6775=AXIS2_PLACEMENT_3D('',#10466,#8050,#8051);
#6776=AXIS2_PLACEMENT_3D('',#10467,#8052,#8053);
#6777=AXIS2_PLACEMENT_3D('',#10468,#8054,#8055);
#6778=AXIS2_PLACEMENT_3D('',#10469,#8056,#8057);
#6779=AXIS2_PLACEMENT_3D('',#10470,#8058,#8059);
#6780=AXIS2_PLACEMENT_3D('',#10472,#8060,#8061);
#6781=AXIS2_PLACEMENT_3D('',#10474,#8063,#8064);
#6782=AXIS2_PLACEMENT_3D('',#10476,#8065,#8066);
#6783=AXIS2_PLACEMENT_3D('',#10478,#8068,#8069);
#6784=AXIS2_PLACEMENT_3D('',#10480,#8070,#8071);
#6785=AXIS2_PLACEMENT_3D('',#10482,#8073,#8074);
#6786=AXIS2_PLACEMENT_3D('',#10484,#8075,#8076);
#6787=AXIS2_PLACEMENT_3D('',#10486,#8078,#8079);
#6788=AXIS2_PLACEMENT_3D('',#10488,#8080,#8081);
#6789=AXIS2_PLACEMENT_3D('',#10490,#8083,#8084);
#6790=AXIS2_PLACEMENT_3D('',#10492,#8085,#8086);
#6791=AXIS2_PLACEMENT_3D('',#10494,#8088,#8089);
#6792=AXIS2_PLACEMENT_3D('',#10496,#8090,#8091);
#6793=AXIS2_PLACEMENT_3D('',#10498,#8092,#8093);
#6794=AXIS2_PLACEMENT_3D('',#10499,#8094,#8095);
#6795=AXIS2_PLACEMENT_3D('',#10501,#8097,#8098);
#6796=AXIS2_PLACEMENT_3D('',#10504,#8100,#8101);
#6797=AXIS2_PLACEMENT_3D('',#10505,#8102,#8103);
#6798=AXIS2_PLACEMENT_3D('',#10506,#8104,#8105);
#6799=AXIS2_PLACEMENT_3D('',#10507,#8106,#8107);
#6800=AXIS2_PLACEMENT_3D('',#10509,#8108,#8109);
#6801=AXIS2_PLACEMENT_3D('',#10512,#8111,#8112);
#6802=AXIS2_PLACEMENT_3D('',#10513,#8113,#8114);
#6803=AXIS2_PLACEMENT_3D('',#10515,#8115,#8116);
#6804=AXIS2_PLACEMENT_3D('',#10518,#8118,#8119);
#6805=AXIS2_PLACEMENT_3D('',#10519,#8120,#8121);
#6806=AXIS2_PLACEMENT_3D('',#10520,#8122,#8123);
#6807=AXIS2_PLACEMENT_3D('',#10521,#8124,#8125);
#6808=AXIS2_PLACEMENT_3D('',#10522,#8126,#8127);
#6809=AXIS2_PLACEMENT_3D('',#10531,#8132,#8133);
#6810=AXIS2_PLACEMENT_3D('',#10538,#8137,#8138);
#6811=AXIS2_PLACEMENT_3D('',#10539,#8139,#8140);
#6812=AXIS2_PLACEMENT_3D('',#10545,#8144,#8145);
#6813=AXIS2_PLACEMENT_3D('',#10547,#8146,#8147);
#6814=AXIS2_PLACEMENT_3D('',#10548,#8148,#8149);
#6815=AXIS2_PLACEMENT_3D('',#10549,#8150,#8151);
#6816=AXIS2_PLACEMENT_3D('',#10550,#8152,#8153);
#6817=AXIS2_PLACEMENT_3D('',#10665,#8154,#8155);
#6818=AXIS2_PLACEMENT_3D('',#10708,#8157,#8158);
#6819=AXIS2_PLACEMENT_3D('',#10751,#8160,#8161);
#6820=AXIS2_PLACEMENT_3D('',#10753,#8162,#8163);
#6821=AXIS2_PLACEMENT_3D('',#10757,#8166,#8167);
#6822=AXIS2_PLACEMENT_3D('',#10840,#8168,#8169);
#6823=AXIS2_PLACEMENT_3D('',#10842,#8171,#8172);
#6824=AXIS2_PLACEMENT_3D('',#10844,#8174,#8175);
#6825=AXIS2_PLACEMENT_3D('',#10845,#8176,#8177);
#6826=AXIS2_PLACEMENT_3D('',#10847,#8178,#8179);
#6827=AXIS2_PLACEMENT_3D('',#10850,#8180,#8181);
#6828=AXIS2_PLACEMENT_3D('',#10852,#8182,#8183);
#6829=AXIS2_PLACEMENT_3D('',#10854,#8184,#8185);
#6830=AXIS2_PLACEMENT_3D('',#10856,#8186,#8187);
#6831=AXIS2_PLACEMENT_3D('',#10858,#8188,#8189);
#6832=AXIS2_PLACEMENT_3D('',#10860,#8190,#8191);
#6833=AXIS2_PLACEMENT_3D('',#10862,#8192,#8193);
#6834=AXIS2_PLACEMENT_3D('',#10864,#8194,#8195);
#6835=AXIS2_PLACEMENT_3D('',#10866,#8196,#8197);
#6836=AXIS2_PLACEMENT_3D('',#10868,#8198,#8199);
#6837=AXIS2_PLACEMENT_3D('',#10870,#8200,#8201);
#6838=AXIS2_PLACEMENT_3D('',#10872,#8202,#8203);
#6839=AXIS2_PLACEMENT_3D('',#10874,#8204,#8205);
#6840=AXIS2_PLACEMENT_3D('',#10876,#8206,#8207);
#6841=AXIS2_PLACEMENT_3D('',#10878,#8208,#8209);
#6842=AXIS2_PLACEMENT_3D('',#10880,#8210,#8211);
#6843=AXIS2_PLACEMENT_3D('',#10882,#8212,#8213);
#6844=AXIS2_PLACEMENT_3D('',#10884,#8214,#8215);
#6845=AXIS2_PLACEMENT_3D('',#10886,#8216,#8217);
#6846=AXIS2_PLACEMENT_3D('',#10888,#8218,#8219);
#6847=AXIS2_PLACEMENT_3D('',#10890,#8220,#8221);
#6848=AXIS2_PLACEMENT_3D('',#10892,#8222,#8223);
#6849=AXIS2_PLACEMENT_3D('',#10894,#8224,#8225);
#6850=AXIS2_PLACEMENT_3D('',#10896,#8226,#8227);
#6851=AXIS2_PLACEMENT_3D('',#10898,#8228,#8229);
#6852=AXIS2_PLACEMENT_3D('',#10900,#8230,#8231);
#6853=AXIS2_PLACEMENT_3D('',#10902,#8232,#8233);
#6854=AXIS2_PLACEMENT_3D('',#10904,#8234,#8235);
#6855=AXIS2_PLACEMENT_3D('',#10906,#8236,#8237);
#6856=AXIS2_PLACEMENT_3D('',#10908,#8238,#8239);
#6857=AXIS2_PLACEMENT_3D('',#10910,#8240,#8241);
#6858=AXIS2_PLACEMENT_3D('',#10912,#8242,#8243);
#6859=AXIS2_PLACEMENT_3D('',#10914,#8244,#8245);
#6860=AXIS2_PLACEMENT_3D('',#10916,#8246,#8247);
#6861=AXIS2_PLACEMENT_3D('',#10918,#8248,#8249);
#6862=AXIS2_PLACEMENT_3D('',#10920,#8250,#8251);
#6863=AXIS2_PLACEMENT_3D('',#10922,#8252,#8253);
#6864=AXIS2_PLACEMENT_3D('',#10924,#8254,#8255);
#6865=AXIS2_PLACEMENT_3D('',#10926,#8256,#8257);
#6866=AXIS2_PLACEMENT_3D('',#10928,#8258,#8259);
#6867=AXIS2_PLACEMENT_3D('',#10930,#8260,#8261);
#6868=AXIS2_PLACEMENT_3D('',#10932,#8262,#8263);
#6869=AXIS2_PLACEMENT_3D('',#10934,#8264,#8265);
#6870=AXIS2_PLACEMENT_3D('',#10936,#8266,#8267);
#6871=AXIS2_PLACEMENT_3D('',#10938,#8268,#8269);
#6872=AXIS2_PLACEMENT_3D('',#10940,#8270,#8271);
#6873=AXIS2_PLACEMENT_3D('',#10942,#8272,#8273);
#6874=AXIS2_PLACEMENT_3D('',#10944,#8274,#8275);
#6875=AXIS2_PLACEMENT_3D('',#10946,#8276,#8277);
#6876=AXIS2_PLACEMENT_3D('',#10948,#8278,#8279);
#6877=AXIS2_PLACEMENT_3D('',#10950,#8280,#8281);
#6878=AXIS2_PLACEMENT_3D('',#10952,#8282,#8283);
#6879=AXIS2_PLACEMENT_3D('',#10954,#8284,#8285);
#6880=AXIS2_PLACEMENT_3D('',#10956,#8286,#8287);
#6881=AXIS2_PLACEMENT_3D('',#10958,#8288,#8289);
#6882=AXIS2_PLACEMENT_3D('',#10960,#8290,#8291);
#6883=AXIS2_PLACEMENT_3D('',#10962,#8292,#8293);
#6884=AXIS2_PLACEMENT_3D('',#10964,#8294,#8295);
#6885=AXIS2_PLACEMENT_3D('',#10966,#8296,#8297);
#6886=AXIS2_PLACEMENT_3D('',#10968,#8298,#8299);
#6887=AXIS2_PLACEMENT_3D('',#10970,#8300,#8301);
#6888=AXIS2_PLACEMENT_3D('',#10972,#8302,#8303);
#6889=AXIS2_PLACEMENT_3D('',#10974,#8304,#8305);
#6890=AXIS2_PLACEMENT_3D('',#10976,#8306,#8307);
#6891=AXIS2_PLACEMENT_3D('',#10978,#8308,#8309);
#6892=AXIS2_PLACEMENT_3D('',#10980,#8310,#8311);
#6893=AXIS2_PLACEMENT_3D('',#10982,#8312,#8313);
#6894=AXIS2_PLACEMENT_3D('',#10984,#8314,#8315);
#6895=AXIS2_PLACEMENT_3D('',#10986,#8316,#8317);
#6896=AXIS2_PLACEMENT_3D('',#10988,#8318,#8319);
#6897=AXIS2_PLACEMENT_3D('',#10990,#8320,#8321);
#6898=AXIS2_PLACEMENT_3D('',#10992,#8322,#8323);
#6899=AXIS2_PLACEMENT_3D('',#10994,#8324,#8325);
#6900=AXIS2_PLACEMENT_3D('',#10996,#8326,#8327);
#6901=AXIS2_PLACEMENT_3D('',#10998,#8328,#8329);
#6902=AXIS2_PLACEMENT_3D('',#11000,#8330,#8331);
#6903=AXIS2_PLACEMENT_3D('',#11002,#8332,#8333);
#6904=AXIS2_PLACEMENT_3D('',#11004,#8334,#8335);
#6905=AXIS2_PLACEMENT_3D('',#11006,#8336,#8337);
#6906=AXIS2_PLACEMENT_3D('',#11007,#8338,#8339);
#6907=AXIS2_PLACEMENT_3D('',#11008,#8340,#8341);
#6908=AXIS2_PLACEMENT_3D('',#11010,#8342,#8343);
#6909=AXIS2_PLACEMENT_3D('',#11012,#8345,#8346);
#6910=AXIS2_PLACEMENT_3D('',#11013,#8347,#8348);
#6911=AXIS2_PLACEMENT_3D('',#11015,#8349,#8350);
#6912=AXIS2_PLACEMENT_3D('',#11018,#8351,#8352);
#6913=AXIS2_PLACEMENT_3D('',#11020,#8353,#8354);
#6914=AXIS2_PLACEMENT_3D('',#11022,#8355,#8356);
#6915=AXIS2_PLACEMENT_3D('',#11024,#8357,#8358);
#6916=AXIS2_PLACEMENT_3D('',#11026,#8359,#8360);
#6917=AXIS2_PLACEMENT_3D('',#11028,#8361,#8362);
#6918=AXIS2_PLACEMENT_3D('',#11030,#8363,#8364);
#6919=AXIS2_PLACEMENT_3D('',#11032,#8365,#8366);
#6920=AXIS2_PLACEMENT_3D('',#11034,#8367,#8368);
#6921=AXIS2_PLACEMENT_3D('',#11036,#8369,#8370);
#6922=AXIS2_PLACEMENT_3D('',#11038,#8371,#8372);
#6923=AXIS2_PLACEMENT_3D('',#11040,#8373,#8374);
#6924=AXIS2_PLACEMENT_3D('',#11042,#8375,#8376);
#6925=AXIS2_PLACEMENT_3D('',#11044,#8377,#8378);
#6926=AXIS2_PLACEMENT_3D('',#11046,#8379,#8380);
#6927=AXIS2_PLACEMENT_3D('',#11048,#8381,#8382);
#6928=AXIS2_PLACEMENT_3D('',#11050,#8383,#8384);
#6929=AXIS2_PLACEMENT_3D('',#11052,#8385,#8386);
#6930=AXIS2_PLACEMENT_3D('',#11054,#8387,#8388);
#6931=AXIS2_PLACEMENT_3D('',#11056,#8389,#8390);
#6932=AXIS2_PLACEMENT_3D('',#11058,#8391,#8392);
#6933=AXIS2_PLACEMENT_3D('',#11060,#8393,#8394);
#6934=AXIS2_PLACEMENT_3D('',#11062,#8395,#8396);
#6935=AXIS2_PLACEMENT_3D('',#11064,#8397,#8398);
#6936=AXIS2_PLACEMENT_3D('',#11066,#8399,#8400);
#6937=AXIS2_PLACEMENT_3D('',#11068,#8401,#8402);
#6938=AXIS2_PLACEMENT_3D('',#11070,#8403,#8404);
#6939=AXIS2_PLACEMENT_3D('',#11072,#8405,#8406);
#6940=AXIS2_PLACEMENT_3D('',#11074,#8407,#8408);
#6941=AXIS2_PLACEMENT_3D('',#11076,#8409,#8410);
#6942=AXIS2_PLACEMENT_3D('',#11078,#8411,#8412);
#6943=AXIS2_PLACEMENT_3D('',#11080,#8413,#8414);
#6944=AXIS2_PLACEMENT_3D('',#11082,#8415,#8416);
#6945=AXIS2_PLACEMENT_3D('',#11084,#8417,#8418);
#6946=AXIS2_PLACEMENT_3D('',#11086,#8419,#8420);
#6947=AXIS2_PLACEMENT_3D('',#11088,#8421,#8422);
#6948=AXIS2_PLACEMENT_3D('',#11090,#8423,#8424);
#6949=AXIS2_PLACEMENT_3D('',#11092,#8425,#8426);
#6950=AXIS2_PLACEMENT_3D('',#11094,#8427,#8428);
#6951=AXIS2_PLACEMENT_3D('',#11096,#8429,#8430);
#6952=AXIS2_PLACEMENT_3D('',#11098,#8431,#8432);
#6953=AXIS2_PLACEMENT_3D('',#11100,#8433,#8434);
#6954=AXIS2_PLACEMENT_3D('',#11102,#8435,#8436);
#6955=AXIS2_PLACEMENT_3D('',#11104,#8437,#8438);
#6956=AXIS2_PLACEMENT_3D('',#11106,#8439,#8440);
#6957=AXIS2_PLACEMENT_3D('',#11108,#8441,#8442);
#6958=AXIS2_PLACEMENT_3D('',#11110,#8443,#8444);
#6959=AXIS2_PLACEMENT_3D('',#11112,#8445,#8446);
#6960=AXIS2_PLACEMENT_3D('',#11114,#8447,#8448);
#6961=AXIS2_PLACEMENT_3D('',#11116,#8449,#8450);
#6962=AXIS2_PLACEMENT_3D('',#11118,#8451,#8452);
#6963=AXIS2_PLACEMENT_3D('',#11120,#8453,#8454);
#6964=AXIS2_PLACEMENT_3D('',#11122,#8455,#8456);
#6965=AXIS2_PLACEMENT_3D('',#11124,#8457,#8458);
#6966=AXIS2_PLACEMENT_3D('',#11126,#8459,#8460);
#6967=AXIS2_PLACEMENT_3D('',#11128,#8461,#8462);
#6968=AXIS2_PLACEMENT_3D('',#11130,#8463,#8464);
#6969=AXIS2_PLACEMENT_3D('',#11132,#8465,#8466);
#6970=AXIS2_PLACEMENT_3D('',#11134,#8467,#8468);
#6971=AXIS2_PLACEMENT_3D('',#11136,#8469,#8470);
#6972=AXIS2_PLACEMENT_3D('',#11138,#8471,#8472);
#6973=AXIS2_PLACEMENT_3D('',#11140,#8473,#8474);
#6974=AXIS2_PLACEMENT_3D('',#11142,#8475,#8476);
#6975=AXIS2_PLACEMENT_3D('',#11144,#8477,#8478);
#6976=AXIS2_PLACEMENT_3D('',#11146,#8479,#8480);
#6977=AXIS2_PLACEMENT_3D('',#11148,#8481,#8482);
#6978=AXIS2_PLACEMENT_3D('',#11150,#8483,#8484);
#6979=AXIS2_PLACEMENT_3D('',#11152,#8485,#8486);
#6980=AXIS2_PLACEMENT_3D('',#11154,#8487,#8488);
#6981=AXIS2_PLACEMENT_3D('',#11156,#8489,#8490);
#6982=AXIS2_PLACEMENT_3D('',#11158,#8491,#8492);
#6983=AXIS2_PLACEMENT_3D('',#11160,#8493,#8494);
#6984=AXIS2_PLACEMENT_3D('',#11162,#8495,#8496);
#6985=AXIS2_PLACEMENT_3D('',#11164,#8497,#8498);
#6986=AXIS2_PLACEMENT_3D('',#11166,#8499,#8500);
#6987=AXIS2_PLACEMENT_3D('',#11168,#8501,#8502);
#6988=AXIS2_PLACEMENT_3D('',#11170,#8503,#8504);
#6989=AXIS2_PLACEMENT_3D('',#11172,#8505,#8506);
#6990=AXIS2_PLACEMENT_3D('',#11174,#8507,#8508);
#6991=AXIS2_PLACEMENT_3D('',#11175,#8509,#8510);
#6992=AXIS2_PLACEMENT_3D('',#11176,#8511,#8512);
#6993=AXIS2_PLACEMENT_3D('',#11178,#8514,#8515);
#6994=AXIS2_PLACEMENT_3D('',#11181,#8518,#8519);
#6995=AXIS2_PLACEMENT_3D('',#11183,#8521,#8522);
#6996=AXIS2_PLACEMENT_3D('',#11185,#8524,#8525);
#6997=AXIS2_PLACEMENT_3D('',#11187,#8527,#8528);
#6998=AXIS2_PLACEMENT_3D('',#11189,#8530,#8531);
#6999=AXIS2_PLACEMENT_3D('',#11191,#8533,#8534);
#7000=AXIS2_PLACEMENT_3D('',#11193,#8536,#8537);
#7001=AXIS2_PLACEMENT_3D('',#11195,#8539,#8540);
#7002=AXIS2_PLACEMENT_3D('',#11197,#8542,#8543);
#7003=AXIS2_PLACEMENT_3D('',#11199,#8545,#8546);
#7004=AXIS2_PLACEMENT_3D('',#11201,#8548,#8549);
#7005=AXIS2_PLACEMENT_3D('',#11203,#8551,#8552);
#7006=AXIS2_PLACEMENT_3D('',#11205,#8554,#8555);
#7007=AXIS2_PLACEMENT_3D('',#11207,#8557,#8558);
#7008=AXIS2_PLACEMENT_3D('',#11209,#8560,#8561);
#7009=AXIS2_PLACEMENT_3D('',#11211,#8563,#8564);
#7010=AXIS2_PLACEMENT_3D('',#11213,#8566,#8567);
#7011=AXIS2_PLACEMENT_3D('',#11215,#8569,#8570);
#7012=AXIS2_PLACEMENT_3D('',#11217,#8572,#8573);
#7013=AXIS2_PLACEMENT_3D('',#11219,#8575,#8576);
#7014=AXIS2_PLACEMENT_3D('',#11221,#8578,#8579);
#7015=AXIS2_PLACEMENT_3D('',#11223,#8581,#8582);
#7016=AXIS2_PLACEMENT_3D('',#11225,#8584,#8585);
#7017=AXIS2_PLACEMENT_3D('',#11227,#8587,#8588);
#7018=AXIS2_PLACEMENT_3D('',#11229,#8590,#8591);
#7019=AXIS2_PLACEMENT_3D('',#11231,#8593,#8594);
#7020=AXIS2_PLACEMENT_3D('',#11233,#8596,#8597);
#7021=AXIS2_PLACEMENT_3D('',#11235,#8599,#8600);
#7022=AXIS2_PLACEMENT_3D('',#11237,#8602,#8603);
#7023=AXIS2_PLACEMENT_3D('',#11239,#8605,#8606);
#7024=AXIS2_PLACEMENT_3D('',#11241,#8608,#8609);
#7025=AXIS2_PLACEMENT_3D('',#11243,#8611,#8612);
#7026=AXIS2_PLACEMENT_3D('',#11245,#8614,#8615);
#7027=AXIS2_PLACEMENT_3D('',#11247,#8617,#8618);
#7028=AXIS2_PLACEMENT_3D('',#11249,#8620,#8621);
#7029=AXIS2_PLACEMENT_3D('',#11251,#8623,#8624);
#7030=AXIS2_PLACEMENT_3D('',#11253,#8626,#8627);
#7031=AXIS2_PLACEMENT_3D('',#11255,#8629,#8630);
#7032=AXIS2_PLACEMENT_3D('',#11257,#8632,#8633);
#7033=AXIS2_PLACEMENT_3D('',#11259,#8635,#8636);
#7034=AXIS2_PLACEMENT_3D('',#11261,#8638,#8639);
#7035=AXIS2_PLACEMENT_3D('',#11263,#8641,#8642);
#7036=AXIS2_PLACEMENT_3D('',#11265,#8644,#8645);
#7037=AXIS2_PLACEMENT_3D('',#11267,#8647,#8648);
#7038=AXIS2_PLACEMENT_3D('',#11269,#8650,#8651);
#7039=AXIS2_PLACEMENT_3D('',#11271,#8653,#8654);
#7040=AXIS2_PLACEMENT_3D('',#11273,#8656,#8657);
#7041=AXIS2_PLACEMENT_3D('',#11275,#8659,#8660);
#7042=AXIS2_PLACEMENT_3D('',#11277,#8662,#8663);
#7043=AXIS2_PLACEMENT_3D('',#11279,#8665,#8666);
#7044=AXIS2_PLACEMENT_3D('',#11281,#8668,#8669);
#7045=AXIS2_PLACEMENT_3D('',#11283,#8671,#8672);
#7046=AXIS2_PLACEMENT_3D('',#11285,#8674,#8675);
#7047=AXIS2_PLACEMENT_3D('',#11287,#8677,#8678);
#7048=AXIS2_PLACEMENT_3D('',#11289,#8680,#8681);
#7049=AXIS2_PLACEMENT_3D('',#11291,#8683,#8684);
#7050=AXIS2_PLACEMENT_3D('',#11293,#8686,#8687);
#7051=AXIS2_PLACEMENT_3D('',#11295,#8689,#8690);
#7052=AXIS2_PLACEMENT_3D('',#11297,#8692,#8693);
#7053=AXIS2_PLACEMENT_3D('',#11299,#8695,#8696);
#7054=AXIS2_PLACEMENT_3D('',#11301,#8698,#8699);
#7055=AXIS2_PLACEMENT_3D('',#11303,#8701,#8702);
#7056=AXIS2_PLACEMENT_3D('',#11305,#8704,#8705);
#7057=AXIS2_PLACEMENT_3D('',#11307,#8707,#8708);
#7058=AXIS2_PLACEMENT_3D('',#11309,#8710,#8711);
#7059=AXIS2_PLACEMENT_3D('',#11311,#8713,#8714);
#7060=AXIS2_PLACEMENT_3D('',#11313,#8716,#8717);
#7061=AXIS2_PLACEMENT_3D('',#11315,#8719,#8720);
#7062=AXIS2_PLACEMENT_3D('',#11317,#8722,#8723);
#7063=AXIS2_PLACEMENT_3D('',#11319,#8725,#8726);
#7064=AXIS2_PLACEMENT_3D('',#11321,#8728,#8729);
#7065=AXIS2_PLACEMENT_3D('',#11323,#8731,#8732);
#7066=AXIS2_PLACEMENT_3D('',#11325,#8734,#8735);
#7067=AXIS2_PLACEMENT_3D('',#11327,#8737,#8738);
#7068=AXIS2_PLACEMENT_3D('',#11329,#8740,#8741);
#7069=AXIS2_PLACEMENT_3D('',#11331,#8743,#8744);
#7070=AXIS2_PLACEMENT_3D('',#11333,#8746,#8747);
#7071=AXIS2_PLACEMENT_3D('',#11335,#8749,#8750);
#7072=AXIS2_PLACEMENT_3D('',#11337,#8752,#8753);
#7073=AXIS2_PLACEMENT_3D('',#11338,#8754,#8755);
#7074=AXIS2_PLACEMENT_3D('',#11339,#8756,#8757);
#7075=AXIS2_PLACEMENT_3D('',#11356,#8766,#8767);
#7076=AXIS2_PLACEMENT_3D('',#11362,#8771,#8772);
#7077=AXIS2_PLACEMENT_3D('',#11366,#8775,#8776);
#7078=AXIS2_PLACEMENT_3D('',#11370,#8779,#8780);
#7079=AXIS2_PLACEMENT_3D('',#11374,#8783,#8784);
#7080=AXIS2_PLACEMENT_3D('',#11382,#8789,#8790);
#7081=AXIS2_PLACEMENT_3D('',#11384,#8792,#8793);
#7082=AXIS2_PLACEMENT_3D('',#11386,#8795,#8796);
#7083=AXIS2_PLACEMENT_3D('',#11388,#8798,#8799);
#7084=AXIS2_PLACEMENT_3D('',#11389,#8800,#8801);
#7085=AXIS2_PLACEMENT_3D('',#11390,#8802,#8803);
#7086=AXIS2_PLACEMENT_3D('',#11392,#8804,#8805);
#7087=AXIS2_PLACEMENT_3D('',#11393,#8806,#8807);
#7088=AXIS2_PLACEMENT_3D('',#11395,#8808,#8809);
#7089=AXIS2_PLACEMENT_3D('',#11397,#8811,#8812);
#7090=AXIS2_PLACEMENT_3D('',#11399,#8813,#8814);
#7091=AXIS2_PLACEMENT_3D('',#11401,#8816,#8817);
#7092=AXIS2_PLACEMENT_3D('',#11403,#8818,#8819);
#7093=AXIS2_PLACEMENT_3D('',#11405,#8821,#8822);
#7094=AXIS2_PLACEMENT_3D('',#11407,#8823,#8824);
#7095=AXIS2_PLACEMENT_3D('',#11408,#8825,#8826);
#7096=AXIS2_PLACEMENT_3D('',#11410,#8827,#8828);
#7097=AXIS2_PLACEMENT_3D('',#11412,#8830,#8831);
#7098=AXIS2_PLACEMENT_3D('',#11414,#8832,#8833);
#7099=AXIS2_PLACEMENT_3D('',#11416,#8835,#8836);
#7100=AXIS2_PLACEMENT_3D('',#11418,#8837,#8838);
#7101=AXIS2_PLACEMENT_3D('',#11420,#8840,#8841);
#7102=AXIS2_PLACEMENT_3D('',#11421,#8842,#8843);
#7103=AXIS2_PLACEMENT_3D('',#11430,#8848,#8849);
#7104=AXIS2_PLACEMENT_3D('',#11436,#8853,#8854);
#7105=AXIS2_PLACEMENT_3D('',#11442,#8858,#8859);
#7106=AXIS2_PLACEMENT_3D('',#11448,#8863,#8864);
#7107=AXIS2_PLACEMENT_3D('',#11454,#8868,#8869);
#7108=AXIS2_PLACEMENT_3D('',#11457,#8872,#8873);
#7109=AXIS2_PLACEMENT_3D('',#11458,#8874,#8875);
#7110=AXIS2_PLACEMENT_3D('',#11459,#8876,#8877);
#7111=AXIS2_PLACEMENT_3D('',#11460,#8878,#8879);
#7112=AXIS2_PLACEMENT_3D('',#11469,#8884,#8885);
#7113=AXIS2_PLACEMENT_3D('',#11475,#8889,#8890);
#7114=AXIS2_PLACEMENT_3D('',#11481,#8894,#8895);
#7115=AXIS2_PLACEMENT_3D('',#11487,#8899,#8900);
#7116=AXIS2_PLACEMENT_3D('',#11493,#8904,#8905);
#7117=AXIS2_PLACEMENT_3D('',#11496,#8908,#8909);
#7118=AXIS2_PLACEMENT_3D('',#11497,#8910,#8911);
#7119=AXIS2_PLACEMENT_3D('',#11499,#8912,#8913);
#7120=AXIS2_PLACEMENT_3D('',#11500,#8914,#8915);
#7121=AXIS2_PLACEMENT_3D('',#11502,#8916,#8917);
#7122=AXIS2_PLACEMENT_3D('',#11504,#8919,#8920);
#7123=AXIS2_PLACEMENT_3D('',#11506,#8921,#8922);
#7124=AXIS2_PLACEMENT_3D('',#11508,#8924,#8925);
#7125=AXIS2_PLACEMENT_3D('',#11510,#8926,#8927);
#7126=AXIS2_PLACEMENT_3D('',#11512,#8929,#8930);
#7127=AXIS2_PLACEMENT_3D('',#11513,#8931,#8932);
#7128=AXIS2_PLACEMENT_3D('',#11514,#8933,#8934);
#7129=AXIS2_PLACEMENT_3D('',#11531,#8943,#8944);
#7130=AXIS2_PLACEMENT_3D('',#11537,#8948,#8949);
#7131=AXIS2_PLACEMENT_3D('',#11541,#8952,#8953);
#7132=AXIS2_PLACEMENT_3D('',#11545,#8956,#8957);
#7133=AXIS2_PLACEMENT_3D('',#11549,#8960,#8961);
#7134=AXIS2_PLACEMENT_3D('',#11557,#8966,#8967);
#7135=AXIS2_PLACEMENT_3D('',#11559,#8969,#8970);
#7136=AXIS2_PLACEMENT_3D('',#11561,#8972,#8973);
#7137=AXIS2_PLACEMENT_3D('',#11563,#8975,#8976);
#7138=AXIS2_PLACEMENT_3D('',#11564,#8977,#8978);
#7139=AXIS2_PLACEMENT_3D('',#11565,#8979,#8980);
#7140=AXIS2_PLACEMENT_3D('',#11567,#8981,#8982);
#7141=AXIS2_PLACEMENT_3D('',#11570,#8984,#8985);
#7142=AXIS2_PLACEMENT_3D('',#11571,#8986,#8987);
#7143=AXIS2_PLACEMENT_3D('',#11573,#8988,#8989);
#7144=AXIS2_PLACEMENT_3D('',#11576,#8991,#8992);
#7145=AXIS2_PLACEMENT_3D('',#11577,#8993,#8994);
#7146=AXIS2_PLACEMENT_3D('',#11578,#8995,#8996);
#7147=AXIS2_PLACEMENT_3D('',#11579,#8997,#8998);
#7148=AXIS2_PLACEMENT_3D('',#11580,#8999,#9000);
#7149=AXIS2_PLACEMENT_3D('',#11592,#9002,#9003);
#7150=AXIS2_PLACEMENT_3D('',#11608,#9004,#9005);
#7151=AXIS2_PLACEMENT_3D('',#11610,#9006,#9007);
#7152=AXIS2_PLACEMENT_3D('',#11636,#9009,#9010);
#7153=AXIS2_PLACEMENT_3D('',#11639,#9013,#9014);
#7154=AXIS2_PLACEMENT_3D('',#11641,#9016,#9017);
#7155=AXIS2_PLACEMENT_3D('',#11643,#9019,#9020);
#7156=AXIS2_PLACEMENT_3D('',#11645,#9021,#9022);
#7157=AXIS2_PLACEMENT_3D('',#11648,#9024,#9025);
#7158=AXIS2_PLACEMENT_3D('',#11649,#9026,#9027);
#7159=AXIS2_PLACEMENT_3D('',#11651,#9029,#9030);
#7160=AXIS2_PLACEMENT_3D('',#11653,#9032,#9033);
#7161=AXIS2_PLACEMENT_3D('',#11654,#9034,#9035);
#7162=AXIS2_PLACEMENT_3D('',#11655,#9036,#9037);
#7163=AXIS2_PLACEMENT_3D('',#11656,#9038,#9039);
#7164=AXIS2_PLACEMENT_3D('',#11657,#9040,#9041);
#7165=AXIS2_PLACEMENT_3D('',#11658,#9042,#9043);
#7166=AXIS2_PLACEMENT_3D('',#11659,#9044,#9045);
#7167=AXIS2_PLACEMENT_3D('',#11660,#9046,#9047);
#7168=AXIS2_PLACEMENT_3D('',#11661,#9048,#9049);
#7169=AXIS2_PLACEMENT_3D('',#11662,#9050,#9051);
#7170=AXIS2_PLACEMENT_3D('',#11663,#9052,#9053);
#7171=AXIS2_PLACEMENT_3D('',#11664,#9054,#9055);
#7172=AXIS2_PLACEMENT_3D('',#11665,#9056,#9057);
#7173=AXIS2_PLACEMENT_3D('',#11666,#9058,#9059);
#7174=AXIS2_PLACEMENT_3D('',#11667,#9060,#9061);
#7175=AXIS2_PLACEMENT_3D('',#11668,#9062,#9063);
#7176=AXIS2_PLACEMENT_3D('',#11669,#9064,#9065);
#7177=AXIS2_PLACEMENT_3D('',#11670,#9066,#9067);
#7178=AXIS2_PLACEMENT_3D('',#11671,#9068,#9069);
#7179=AXIS2_PLACEMENT_3D('',#11672,#9070,#9071);
#7180=AXIS2_PLACEMENT_3D('',#11673,#9072,#9073);
#7181=AXIS2_PLACEMENT_3D('',#11674,#9074,#9075);
#7182=AXIS2_PLACEMENT_3D('',#11675,#9076,#9077);
#7183=AXIS2_PLACEMENT_3D('',#11676,#9078,#9079);
#7184=AXIS2_PLACEMENT_3D('',#11677,#9080,#9081);
#7185=AXIS2_PLACEMENT_3D('',#11678,#9082,#9083);
#7186=AXIS2_PLACEMENT_3D('',#11679,#9084,#9085);
#7187=AXIS2_PLACEMENT_3D('',#11680,#9086,#9087);
#7188=AXIS2_PLACEMENT_3D('',#11681,#9088,#9089);
#7189=AXIS2_PLACEMENT_3D('',#11682,#9090,#9091);
#7190=AXIS2_PLACEMENT_3D('',#11683,#9092,#9093);
#7191=AXIS2_PLACEMENT_3D('',#11684,#9094,#9095);
#7192=AXIS2_PLACEMENT_3D('',#11685,#9096,#9097);
#7193=AXIS2_PLACEMENT_3D('',#11686,#9098,#9099);
#7194=AXIS2_PLACEMENT_3D('',#11687,#9100,#9101);
#7195=AXIS2_PLACEMENT_3D('',#11688,#9102,#9103);
#7196=AXIS2_PLACEMENT_3D('',#11689,#9104,#9105);
#7197=AXIS2_PLACEMENT_3D('',#11690,#9106,#9107);
#7198=AXIS2_PLACEMENT_3D('',#11691,#9108,#9109);
#7199=AXIS2_PLACEMENT_3D('',#11692,#9110,#9111);
#7200=AXIS2_PLACEMENT_3D('',#11693,#9112,#9113);
#7201=AXIS2_PLACEMENT_3D('',#11694,#9114,#9115);
#7202=AXIS2_PLACEMENT_3D('',#11695,#9116,#9117);
#7203=AXIS2_PLACEMENT_3D('',#11696,#9118,#9119);
#7204=AXIS2_PLACEMENT_3D('',#11697,#9120,#9121);
#7205=AXIS2_PLACEMENT_3D('',#11698,#9122,#9123);
#7206=AXIS2_PLACEMENT_3D('',#11699,#9124,#9125);
#7207=AXIS2_PLACEMENT_3D('',#11700,#9126,#9127);
#7208=DIRECTION('axis',(0.,0.,1.));
#7209=DIRECTION('refdir',(1.,0.,0.));
#7210=DIRECTION('axis',(0.,0.,1.));
#7211=DIRECTION('refdir',(1.,0.,0.));
#7212=DIRECTION('axis',(0.,0.,1.));
#7213=DIRECTION('refdir',(1.,0.,0.));
#7214=DIRECTION('center_axis',(0.,0.,1.));
#7215=DIRECTION('ref_axis',(1.,0.,0.));
#7216=DIRECTION('center_axis',(0.,0.,1.));
#7217=DIRECTION('ref_axis',(1.,0.,0.));
#7218=DIRECTION('',(0.,0.,1.));
#7219=DIRECTION('center_axis',(0.,0.,-1.));
#7220=DIRECTION('ref_axis',(1.,0.,0.));
#7221=DIRECTION('center_axis',(0.,0.,1.));
#7222=DIRECTION('ref_axis',(1.,0.,0.));
#7223=DIRECTION('center_axis',(0.,0.,1.));
#7224=DIRECTION('ref_axis',(1.,0.,0.));
#7225=DIRECTION('',(0.,0.,1.));
#7226=DIRECTION('center_axis',(0.,0.,-1.));
#7227=DIRECTION('ref_axis',(1.,0.,0.));
#7228=DIRECTION('center_axis',(0.,1.,0.));
#7229=DIRECTION('ref_axis',(-1.,0.,0.));
#7230=DIRECTION('',(-1.,0.,0.));
#7231=DIRECTION('',(0.,0.,1.));
#7232=DIRECTION('',(-1.,0.,0.));
#7233=DIRECTION('',(0.,0.,1.));
#7234=DIRECTION('center_axis',(1.,0.,0.));
#7235=DIRECTION('ref_axis',(0.,1.,0.));
#7236=DIRECTION('',(0.,1.,0.));
#7237=DIRECTION('',(0.,1.,0.));
#7238=DIRECTION('',(0.,0.,1.));
#7239=DIRECTION('center_axis',(0.,-1.,0.));
#7240=DIRECTION('ref_axis',(1.,0.,0.));
#7241=DIRECTION('',(1.,0.,0.));
#7242=DIRECTION('',(1.,0.,0.));
#7243=DIRECTION('',(0.,0.,1.));
#7244=DIRECTION('center_axis',(-1.,0.,0.));
#7245=DIRECTION('ref_axis',(0.,-1.,0.));
#7246=DIRECTION('',(0.,-1.,0.));
#7247=DIRECTION('',(0.,-1.,0.));
#7248=DIRECTION('center_axis',(0.,0.,1.));
#7249=DIRECTION('ref_axis',(1.,0.,0.));
#7250=DIRECTION('center_axis',(0.,0.,1.));
#7251=DIRECTION('ref_axis',(1.,0.,0.));
#7252=DIRECTION('axis',(0.,0.,1.));
#7253=DIRECTION('refdir',(1.,0.,0.));
#7254=DIRECTION('center_axis',(0.,0.,1.));
#7255=DIRECTION('ref_axis',(1.,0.,0.));
#7256=DIRECTION('center_axis',(0.,0.,1.));
#7257=DIRECTION('ref_axis',(1.,0.,0.));
#7258=DIRECTION('',(0.,0.,1.));
#7259=DIRECTION('center_axis',(0.,0.,-1.));
#7260=DIRECTION('ref_axis',(1.,0.,0.));
#7261=DIRECTION('center_axis',(0.,0.,1.));
#7262=DIRECTION('ref_axis',(1.,0.,0.));
#7263=DIRECTION('center_axis',(0.,0.,1.));
#7264=DIRECTION('ref_axis',(1.,0.,0.));
#7265=DIRECTION('',(0.,0.,1.));
#7266=DIRECTION('center_axis',(0.,0.,-1.));
#7267=DIRECTION('ref_axis',(1.,0.,0.));
#7268=DIRECTION('center_axis',(0.,1.,0.));
#7269=DIRECTION('ref_axis',(1.,0.,0.));
#7270=DIRECTION('center_axis',(0.,1.,0.));
#7271=DIRECTION('ref_axis',(1.,0.,0.));
#7272=DIRECTION('',(0.,1.,0.));
#7273=DIRECTION('center_axis',(0.,-1.,0.));
#7274=DIRECTION('ref_axis',(1.,0.,0.));
#7275=DIRECTION('center_axis',(0.,1.,0.));
#7276=DIRECTION('ref_axis',(1.,0.,0.));
#7277=DIRECTION('center_axis',(0.,1.,0.));
#7278=DIRECTION('ref_axis',(1.,0.,0.));
#7279=DIRECTION('',(0.,1.,0.));
#7280=DIRECTION('center_axis',(0.,-1.,0.));
#7281=DIRECTION('ref_axis',(1.,0.,0.));
#7282=DIRECTION('center_axis',(0.,1.,0.));
#7283=DIRECTION('ref_axis',(1.,0.,0.));
#7284=DIRECTION('center_axis',(0.,1.,0.));
#7285=DIRECTION('ref_axis',(1.,0.,0.));
#7286=DIRECTION('',(0.,1.,0.));
#7287=DIRECTION('center_axis',(0.,-1.,0.));
#7288=DIRECTION('ref_axis',(1.,0.,0.));
#7289=DIRECTION('center_axis',(0.,1.,0.));
#7290=DIRECTION('ref_axis',(1.,0.,0.));
#7291=DIRECTION('center_axis',(0.,1.,0.));
#7292=DIRECTION('ref_axis',(1.,0.,0.));
#7293=DIRECTION('',(0.,1.,0.));
#7294=DIRECTION('center_axis',(0.,-1.,0.));
#7295=DIRECTION('ref_axis',(1.,0.,0.));
#7296=DIRECTION('center_axis',(0.,1.,0.));
#7297=DIRECTION('ref_axis',(1.,0.,0.));
#7298=DIRECTION('center_axis',(0.,1.,0.));
#7299=DIRECTION('ref_axis',(1.,0.,0.));
#7300=DIRECTION('',(0.,1.,0.));
#7301=DIRECTION('center_axis',(0.,-1.,0.));
#7302=DIRECTION('ref_axis',(1.,0.,0.));
#7303=DIRECTION('center_axis',(0.,0.,1.));
#7304=DIRECTION('ref_axis',(1.,0.,0.));
#7305=DIRECTION('',(1.,0.,0.));
#7306=DIRECTION('',(0.,1.,0.));
#7307=DIRECTION('',(-1.,0.,0.));
#7308=DIRECTION('',(0.,1.,0.));
#7309=DIRECTION('center_axis',(0.,1.,0.));
#7310=DIRECTION('ref_axis',(1.,0.,0.));
#7311=DIRECTION('',(0.,0.,-1.));
#7312=DIRECTION('',(1.,0.,0.));
#7313=DIRECTION('',(0.,0.,1.));
#7314=DIRECTION('center_axis',(0.,1.,0.));
#7315=DIRECTION('ref_axis',(-1.,0.,0.));
#7316=DIRECTION('',(0.,0.,1.));
#7317=DIRECTION('',(-1.,0.,0.));
#7318=DIRECTION('',(0.,0.,1.));
#7319=DIRECTION('',(-1.,0.,0.));
#7320=DIRECTION('center_axis',(-1.,0.,0.));
#7321=DIRECTION('ref_axis',(0.,-1.,0.));
#7322=DIRECTION('',(0.,0.,1.));
#7323=DIRECTION('',(0.,-1.,0.));
#7324=DIRECTION('',(0.,-1.,0.));
#7325=DIRECTION('center_axis',(1.,0.,0.));
#7326=DIRECTION('ref_axis',(0.,1.,0.));
#7327=DIRECTION('',(0.,1.,0.));
#7328=DIRECTION('',(0.,0.,1.));
#7329=DIRECTION('',(0.,1.,0.));
#7330=DIRECTION('center_axis',(0.,-1.,0.));
#7331=DIRECTION('ref_axis',(1.,0.,0.));
#7332=DIRECTION('',(1.,0.,0.));
#7333=DIRECTION('center_axis',(0.,0.,1.));
#7334=DIRECTION('ref_axis',(1.,0.,0.));
#7335=DIRECTION('center_axis',(0.,0.,1.));
#7336=DIRECTION('ref_axis',(1.,0.,0.));
#7337=DIRECTION('axis',(0.,0.,1.));
#7338=DIRECTION('refdir',(1.,0.,0.));
#7339=DIRECTION('center_axis',(0.,1.,0.));
#7340=DIRECTION('ref_axis',(1.,0.,0.));
#7341=DIRECTION('center_axis',(0.,-1.,0.));
#7342=DIRECTION('ref_axis',(1.,0.,0.));
#7343=DIRECTION('',(0.,-1.,0.));
#7344=DIRECTION('center_axis',(0.,-1.,0.));
#7345=DIRECTION('ref_axis',(1.,0.,0.));
#7346=DIRECTION('center_axis',(0.,1.,0.));
#7347=DIRECTION('ref_axis',(1.,0.,0.));
#7348=DIRECTION('center_axis',(0.,1.,0.));
#7349=DIRECTION('ref_axis',(1.,0.,0.));
#7350=DIRECTION('',(0.,-1.,0.));
#7351=DIRECTION('center_axis',(0.,1.,0.));
#7352=DIRECTION('ref_axis',(1.,0.,0.));
#7353=DIRECTION('center_axis',(0.,1.,0.));
#7354=DIRECTION('ref_axis',(1.,0.,0.));
#7355=DIRECTION('center_axis',(0.,1.,0.));
#7356=DIRECTION('ref_axis',(1.,0.,0.));
#7357=DIRECTION('axis',(0.,0.,1.));
#7358=DIRECTION('refdir',(1.,0.,0.));
#7359=DIRECTION('center_axis',(0.,1.,0.));
#7360=DIRECTION('ref_axis',(1.,0.,0.));
#7361=DIRECTION('center_axis',(0.,-1.,0.));
#7362=DIRECTION('ref_axis',(1.,0.,0.));
#7363=DIRECTION('',(0.,-1.,0.));
#7364=DIRECTION('center_axis',(0.,-1.,0.));
#7365=DIRECTION('ref_axis',(1.,0.,0.));
#7366=DIRECTION('center_axis',(0.,1.,0.));
#7367=DIRECTION('ref_axis',(1.,0.,0.));
#7368=DIRECTION('center_axis',(0.,1.,0.));
#7369=DIRECTION('ref_axis',(1.,0.,0.));
#7370=DIRECTION('',(0.,-1.,0.));
#7371=DIRECTION('center_axis',(0.,1.,0.));
#7372=DIRECTION('ref_axis',(1.,0.,0.));
#7373=DIRECTION('center_axis',(0.,1.,0.));
#7374=DIRECTION('ref_axis',(1.,0.,0.));
#7375=DIRECTION('center_axis',(0.,1.,0.));
#7376=DIRECTION('ref_axis',(1.,0.,0.));
#7377=DIRECTION('axis',(0.,0.,1.));
#7378=DIRECTION('refdir',(1.,0.,0.));
#7379=DIRECTION('center_axis',(0.,1.,0.));
#7380=DIRECTION('ref_axis',(1.,0.,0.));
#7381=DIRECTION('center_axis',(0.,-1.,0.));
#7382=DIRECTION('ref_axis',(1.,0.,0.));
#7383=DIRECTION('',(0.,-1.,0.));
#7384=DIRECTION('center_axis',(0.,-1.,0.));
#7385=DIRECTION('ref_axis',(1.,0.,0.));
#7386=DIRECTION('center_axis',(0.,1.,0.));
#7387=DIRECTION('ref_axis',(1.,0.,0.));
#7388=DIRECTION('center_axis',(0.,1.,0.));
#7389=DIRECTION('ref_axis',(1.,0.,0.));
#7390=DIRECTION('',(0.,-1.,0.));
#7391=DIRECTION('center_axis',(0.,1.,0.));
#7392=DIRECTION('ref_axis',(1.,0.,0.));
#7393=DIRECTION('center_axis',(0.,1.,0.));
#7394=DIRECTION('ref_axis',(1.,0.,0.));
#7395=DIRECTION('center_axis',(0.,1.,0.));
#7396=DIRECTION('ref_axis',(1.,0.,0.));
#7397=DIRECTION('axis',(0.,0.,1.));
#7398=DIRECTION('refdir',(1.,0.,0.));
#7399=DIRECTION('center_axis',(0.,1.,0.));
#7400=DIRECTION('ref_axis',(1.,0.,0.));
#7401=DIRECTION('center_axis',(0.,-1.,0.));
#7402=DIRECTION('ref_axis',(1.,0.,0.));
#7403=DIRECTION('',(0.,-1.,0.));
#7404=DIRECTION('center_axis',(0.,-1.,0.));
#7405=DIRECTION('ref_axis',(1.,0.,0.));
#7406=DIRECTION('center_axis',(0.,1.,0.));
#7407=DIRECTION('ref_axis',(1.,0.,0.));
#7408=DIRECTION('center_axis',(0.,1.,0.));
#7409=DIRECTION('ref_axis',(1.,0.,0.));
#7410=DIRECTION('',(0.,-1.,0.));
#7411=DIRECTION('center_axis',(0.,1.,0.));
#7412=DIRECTION('ref_axis',(1.,0.,0.));
#7413=DIRECTION('center_axis',(0.,1.,0.));
#7414=DIRECTION('ref_axis',(1.,0.,0.));
#7415=DIRECTION('center_axis',(0.,1.,0.));
#7416=DIRECTION('ref_axis',(1.,0.,0.));
#7417=DIRECTION('axis',(0.,0.,1.));
#7418=DIRECTION('refdir',(1.,0.,0.));
#7419=DIRECTION('center_axis',(0.,1.,0.));
#7420=DIRECTION('ref_axis',(-1.,0.,0.));
#7421=DIRECTION('',(-1.,0.,0.));
#7422=DIRECTION('',(0.,0.,1.));
#7423=DIRECTION('',(-1.,0.,0.));
#7424=DIRECTION('',(0.,0.,1.));
#7425=DIRECTION('center_axis',(1.,0.,0.));
#7426=DIRECTION('ref_axis',(0.,1.,0.));
#7427=DIRECTION('',(0.,1.,0.));
#7428=DIRECTION('',(0.,1.,0.));
#7429=DIRECTION('',(0.,0.,1.));
#7430=DIRECTION('center_axis',(0.,-1.,0.));
#7431=DIRECTION('ref_axis',(1.,0.,0.));
#7432=DIRECTION('',(1.,0.,0.));
#7433=DIRECTION('',(1.,0.,0.));
#7434=DIRECTION('',(0.,0.,1.));
#7435=DIRECTION('center_axis',(-1.,0.,0.));
#7436=DIRECTION('ref_axis',(0.,-1.,0.));
#7437=DIRECTION('',(0.,-1.,0.));
#7438=DIRECTION('',(0.,-1.,0.));
#7439=DIRECTION('center_axis',(0.,0.,1.));
#7440=DIRECTION('ref_axis',(1.,0.,0.));
#7441=DIRECTION('center_axis',(0.,0.,1.));
#7442=DIRECTION('ref_axis',(1.,0.,0.));
#7443=DIRECTION('axis',(0.,0.,1.));
#7444=DIRECTION('refdir',(1.,0.,0.));
#7445=DIRECTION('center_axis',(0.,1.,0.));
#7446=DIRECTION('ref_axis',(-1.,0.,0.));
#7447=DIRECTION('',(-1.,0.,0.));
#7448=DIRECTION('',(0.,0.,1.));
#7449=DIRECTION('',(-1.,0.,0.));
#7450=DIRECTION('',(0.,0.,1.));
#7451=DIRECTION('center_axis',(1.,0.,0.));
#7452=DIRECTION('ref_axis',(0.,1.,0.));
#7453=DIRECTION('',(0.,1.,0.));
#7454=DIRECTION('',(0.,1.,0.));
#7455=DIRECTION('',(0.,0.,1.));
#7456=DIRECTION('center_axis',(0.,-1.,0.));
#7457=DIRECTION('ref_axis',(1.,0.,0.));
#7458=DIRECTION('',(1.,0.,0.));
#7459=DIRECTION('',(1.,0.,0.));
#7460=DIRECTION('',(0.,0.,1.));
#7461=DIRECTION('center_axis',(-1.,0.,0.));
#7462=DIRECTION('ref_axis',(0.,-1.,0.));
#7463=DIRECTION('',(0.,-1.,0.));
#7464=DIRECTION('',(0.,-1.,0.));
#7465=DIRECTION('center_axis',(0.,0.,1.));
#7466=DIRECTION('ref_axis',(1.,0.,0.));
#7467=DIRECTION('center_axis',(0.,0.,1.));
#7468=DIRECTION('ref_axis',(1.,0.,0.));
#7469=DIRECTION('axis',(0.,0.,1.));
#7470=DIRECTION('refdir',(1.,0.,0.));
#7471=DIRECTION('center_axis',(0.866025403784439,0.,-0.5));
#7472=DIRECTION('ref_axis',(0.5,0.,0.866025403784439));
#7473=DIRECTION('',(-0.5,0.,-0.866025403784439));
#7474=DIRECTION('',(0.,-1.,0.));
#7475=DIRECTION('',(0.5,0.,0.866025403784439));
#7476=DIRECTION('',(0.,-1.,0.));
#7477=DIRECTION('center_axis',(1.92296268638356E-16,0.,-1.));
#7478=DIRECTION('ref_axis',(1.,0.,1.92296268638356E-16));
#7479=DIRECTION('',(-1.,0.,-1.92296268638356E-16));
#7480=DIRECTION('',(0.,-1.,0.));
#7481=DIRECTION('',(1.,0.,1.92296268638356E-16));
#7482=DIRECTION('center_axis',(-0.866025403784439,0.,-0.5));
#7483=DIRECTION('ref_axis',(0.5,0.,-0.866025403784439));
#7484=DIRECTION('',(-0.5,0.,0.866025403784438));
#7485=DIRECTION('',(0.,-1.,0.));
#7486=DIRECTION('',(0.5,0.,-0.866025403784438));
#7487=DIRECTION('center_axis',(-0.866025403784439,0.,0.5));
#7488=DIRECTION('ref_axis',(-0.5,0.,-0.866025403784439));
#7489=DIRECTION('',(0.5,0.,0.866025403784439));
#7490=DIRECTION('',(0.,-1.,0.));
#7491=DIRECTION('',(-0.5,0.,-0.866025403784439));
#7492=DIRECTION('center_axis',(-1.92296268638356E-16,0.,1.));
#7493=DIRECTION('ref_axis',(-1.,0.,-1.92296268638356E-16));
#7494=DIRECTION('',(1.,0.,1.92296268638356E-16));
#7495=DIRECTION('',(0.,-1.,0.));
#7496=DIRECTION('',(-1.,0.,-1.92296268638356E-16));
#7497=DIRECTION('center_axis',(0.866025403784439,0.,0.5));
#7498=DIRECTION('ref_axis',(-0.5,0.,0.866025403784439));
#7499=DIRECTION('',(0.5,0.,-0.866025403784439));
#7500=DIRECTION('',(-0.5,0.,0.866025403784439));
#7501=DIRECTION('center_axis',(0.,1.,0.));
#7502=DIRECTION('ref_axis',(1.,0.,0.));
#7503=DIRECTION('center_axis',(0.,-1.,0.));
#7504=DIRECTION('ref_axis',(0.,0.,-1.));
#7505=DIRECTION('center_axis',(0.,1.,0.));
#7506=DIRECTION('ref_axis',(1.,0.,0.));
#7507=DIRECTION('center_axis',(0.,1.,0.));
#7508=DIRECTION('ref_axis',(1.,0.,0.));
#7509=DIRECTION('center_axis',(0.,1.,0.));
#7510=DIRECTION('ref_axis',(0.,0.,1.));
#7511=DIRECTION('center_axis',(0.,-1.,0.));
#7512=DIRECTION('ref_axis',(1.,0.,0.));
#7513=DIRECTION('center_axis',(0.,-1.,0.));
#7514=DIRECTION('ref_axis',(1.,0.,0.));
#7515=DIRECTION('center_axis',(0.,-1.,0.));
#7516=DIRECTION('ref_axis',(1.,0.,0.));
#7517=DIRECTION('',(0.707106781186548,0.707106781186547,8.65956056235494E-17));
#7518=DIRECTION('center_axis',(0.,-1.,0.));
#7519=DIRECTION('ref_axis',(1.,0.,0.));
#7520=DIRECTION('center_axis',(0.,-1.,0.));
#7521=DIRECTION('ref_axis',(1.,0.,0.));
#7522=DIRECTION('',(0.,1.,0.));
#7523=DIRECTION('center_axis',(0.,1.,0.));
#7524=DIRECTION('ref_axis',(1.,0.,0.));
#7525=DIRECTION('center_axis',(0.,-1.,0.));
#7526=DIRECTION('ref_axis',(1.,0.,0.));
#7527=DIRECTION('',(-0.707106781186547,0.707106781186548,-8.65956056235493E-17));
#7528=DIRECTION('center_axis',(0.,-1.,0.));
#7529=DIRECTION('ref_axis',(0.,0.,-1.));
#7530=DIRECTION('center_axis',(0.,-1.,0.));
#7531=DIRECTION('ref_axis',(1.,0.,0.));
#7532=DIRECTION('center_axis',(0.,1.,0.));
#7533=DIRECTION('ref_axis',(1.,0.,0.));
#7534=DIRECTION('center_axis',(0.,1.,0.));
#7535=DIRECTION('ref_axis',(1.,0.,0.));
#7536=DIRECTION('',(-0.447213595499958,0.894427190999916,-5.47678698264203E-17));
#7537=DIRECTION('center_axis',(0.,-1.,0.));
#7538=DIRECTION('ref_axis',(1.,0.,0.));
#7539=DIRECTION('',(0.,1.,0.));
#7540=DIRECTION('axis',(0.,0.,1.));
#7541=DIRECTION('refdir',(1.,0.,0.));
#7542=DIRECTION('axis',(0.,0.,1.));
#7543=DIRECTION('refdir',(1.,0.,0.));
#7544=DIRECTION('center_axis',(0.,1.,0.));
#7545=DIRECTION('ref_axis',(1.,0.,0.));
#7546=DIRECTION('center_axis',(0.,1.,0.));
#7547=DIRECTION('ref_axis',(1.,0.,0.));
#7548=DIRECTION('',(0.,1.,0.));
#7549=DIRECTION('center_axis',(0.,-1.,0.));
#7550=DIRECTION('ref_axis',(1.,0.,0.));
#7551=DIRECTION('center_axis',(0.,1.,0.));
#7552=DIRECTION('ref_axis',(1.,0.,0.));
#7553=DIRECTION('center_axis',(0.,1.,0.));
#7554=DIRECTION('ref_axis',(1.,0.,0.));
#7555=DIRECTION('',(0.,1.,0.));
#7556=DIRECTION('center_axis',(0.,-1.,0.));
#7557=DIRECTION('ref_axis',(1.,0.,0.));
#7558=DIRECTION('center_axis',(6.12323399573677E-17,0.,1.));
#7559=DIRECTION('ref_axis',(1.,0.,0.));
#7560=DIRECTION('center_axis',(-1.22464679914735E-16,1.,0.));
#7561=DIRECTION('ref_axis',(-1.,-1.22464679914735E-16,0.));
#7562=DIRECTION('center_axis',(0.,1.,0.));
#7563=DIRECTION('ref_axis',(1.,0.,0.));
#7564=DIRECTION('center_axis',(0.,1.,0.));
#7565=DIRECTION('ref_axis',(1.,0.,0.));
#7566=DIRECTION('',(0.,-1.,0.));
#7567=DIRECTION('center_axis',(0.,-1.,0.));
#7568=DIRECTION('ref_axis',(1.,0.,0.));
#7569=DIRECTION('center_axis',(0.,1.,0.));
#7570=DIRECTION('ref_axis',(1.,0.,0.));
#7571=DIRECTION('center_axis',(0.,1.,0.));
#7572=DIRECTION('ref_axis',(1.,0.,0.));
#7573=DIRECTION('',(0.,-1.,0.));
#7574=DIRECTION('center_axis',(0.,-1.,0.));
#7575=DIRECTION('ref_axis',(1.,0.,0.));
#7576=DIRECTION('center_axis',(0.,1.,0.));
#7577=DIRECTION('ref_axis',(1.,0.,0.));
#7578=DIRECTION('center_axis',(0.,1.,0.));
#7579=DIRECTION('ref_axis',(1.,0.,0.));
#7580=DIRECTION('center_axis',(0.,1.,0.));
#7581=DIRECTION('ref_axis',(1.,0.,0.));
#7582=DIRECTION('center_axis',(0.,1.,0.));
#7583=DIRECTION('ref_axis',(1.,0.,0.));
#7584=DIRECTION('',(0.,1.,0.));
#7585=DIRECTION('center_axis',(0.,-1.,0.));
#7586=DIRECTION('ref_axis',(1.,0.,0.));
#7587=DIRECTION('center_axis',(0.,1.,0.));
#7588=DIRECTION('ref_axis',(1.,0.,0.));
#7589=DIRECTION('center_axis',(0.,1.,0.));
#7590=DIRECTION('ref_axis',(1.,0.,0.));
#7591=DIRECTION('',(0.,1.,0.));
#7592=DIRECTION('center_axis',(0.,-1.,0.));
#7593=DIRECTION('ref_axis',(1.,0.,0.));
#7594=DIRECTION('center_axis',(0.,1.,0.));
#7595=DIRECTION('ref_axis',(1.,0.,0.));
#7596=DIRECTION('center_axis',(0.,1.,0.));
#7597=DIRECTION('ref_axis',(1.,0.,0.));
#7598=DIRECTION('',(0.,1.,0.));
#7599=DIRECTION('center_axis',(0.,-1.,0.));
#7600=DIRECTION('ref_axis',(1.,0.,0.));
#7601=DIRECTION('center_axis',(0.,1.,0.));
#7602=DIRECTION('ref_axis',(1.,0.,0.));
#7603=DIRECTION('center_axis',(0.,1.,0.));
#7604=DIRECTION('ref_axis',(1.,0.,0.));
#7605=DIRECTION('',(0.,1.,0.));
#7606=DIRECTION('center_axis',(0.,-1.,0.));
#7607=DIRECTION('ref_axis',(1.,0.,0.));
#7608=DIRECTION('center_axis',(-1.,0.,0.));
#7609=DIRECTION('ref_axis',(0.,0.,1.));
#7610=DIRECTION('',(0.,0.,1.));
#7611=DIRECTION('',(0.,1.,0.));
#7612=DIRECTION('',(0.,0.,1.));
#7613=DIRECTION('',(0.,1.,0.));
#7614=DIRECTION('center_axis',(-0.707106781186548,0.,-0.707106781186548));
#7615=DIRECTION('ref_axis',(-0.707106781186548,0.,0.707106781186548));
#7616=DIRECTION('',(-0.707106781186548,0.,0.707106781186548));
#7617=DIRECTION('',(-0.707106781186548,0.,0.707106781186548));
#7618=DIRECTION('',(0.,1.,0.));
#7619=DIRECTION('center_axis',(0.,0.,-1.));
#7620=DIRECTION('ref_axis',(-1.,0.,0.));
#7621=DIRECTION('',(-1.,0.,0.));
#7622=DIRECTION('',(-1.,0.,0.));
#7623=DIRECTION('',(0.,1.,0.));
#7624=DIRECTION('center_axis',(0.707106781186548,0.,-0.707106781186548));
#7625=DIRECTION('ref_axis',(-0.707106781186548,0.,-0.707106781186548));
#7626=DIRECTION('',(-0.707106781186548,0.,-0.707106781186548));
#7627=DIRECTION('',(-0.707106781186548,0.,-0.707106781186548));
#7628=DIRECTION('',(0.,1.,0.));
#7629=DIRECTION('center_axis',(1.,0.,0.));
#7630=DIRECTION('ref_axis',(0.,0.,-1.));
#7631=DIRECTION('',(0.,0.,-1.));
#7632=DIRECTION('',(0.,0.,-1.));
#7633=DIRECTION('',(0.,1.,0.));
#7634=DIRECTION('center_axis',(0.707106781186548,0.,0.707106781186548));
#7635=DIRECTION('ref_axis',(0.707106781186548,0.,-0.707106781186548));
#7636=DIRECTION('',(0.707106781186548,0.,-0.707106781186548));
#7637=DIRECTION('',(0.707106781186548,0.,-0.707106781186548));
#7638=DIRECTION('',(0.,1.,0.));
#7639=DIRECTION('center_axis',(0.,0.,1.));
#7640=DIRECTION('ref_axis',(1.,0.,0.));
#7641=DIRECTION('',(1.,0.,0.));
#7642=DIRECTION('',(1.,0.,0.));
#7643=DIRECTION('',(0.,1.,0.));
#7644=DIRECTION('center_axis',(-0.707106781186548,0.,0.707106781186548));
#7645=DIRECTION('ref_axis',(0.707106781186548,0.,0.707106781186548));
#7646=DIRECTION('',(0.707106781186548,0.,0.707106781186548));
#7647=DIRECTION('',(0.707106781186548,0.,0.707106781186548));
#7648=DIRECTION('center_axis',(0.,1.,0.));
#7649=DIRECTION('ref_axis',(0.,0.,1.));
#7650=DIRECTION('center_axis',(0.,1.,0.));
#7651=DIRECTION('ref_axis',(1.,0.,0.));
#7652=DIRECTION('axis',(0.,0.,1.));
#7653=DIRECTION('refdir',(1.,0.,0.));
#7654=DIRECTION('center_axis',(0.,-1.,0.));
#7655=DIRECTION('ref_axis',(1.,0.,0.));
#7656=DIRECTION('center_axis',(0.,-1.,0.));
#7657=DIRECTION('ref_axis',(1.,0.,0.));
#7658=DIRECTION('',(0.,1.,0.));
#7659=DIRECTION('center_axis',(0.,-1.,0.));
#7660=DIRECTION('ref_axis',(1.,0.,0.));
#7661=DIRECTION('center_axis',(0.,1.,0.));
#7662=DIRECTION('ref_axis',(0.,0.,1.));
#7663=DIRECTION('center_axis',(0.,-1.,0.));
#7664=DIRECTION('ref_axis',(1.,0.,0.));
#7665=DIRECTION('center_axis',(6.12323399573677E-17,0.,1.));
#7666=DIRECTION('ref_axis',(1.,0.,0.));
#7667=DIRECTION('center_axis',(1.22464679914735E-16,-1.,0.));
#7668=DIRECTION('ref_axis',(-1.,-1.22464679914735E-16,0.));
#7669=DIRECTION('center_axis',(0.,-1.,0.));
#7670=DIRECTION('ref_axis',(1.,0.,0.));
#7671=DIRECTION('center_axis',(0.,-1.,0.));
#7672=DIRECTION('ref_axis',(0.,0.,-1.));
#7673=DIRECTION('center_axis',(-0.866025403784438,0.,-0.5));
#7674=DIRECTION('ref_axis',(-0.5,0.,0.866025403784438));
#7675=DIRECTION('',(-0.866025403784438,0.,-0.5));
#7676=DIRECTION('center_axis',(-0.866025403784438,0.,-0.5));
#7677=DIRECTION('ref_axis',(-0.5,0.,0.866025403784438));
#7678=DIRECTION('',(-0.866025403784438,0.,-0.5));
#7679=DIRECTION('center_axis',(0.,-1.,0.));
#7680=DIRECTION('ref_axis',(1.,0.,0.));
#7681=DIRECTION('center_axis',(0.,-1.,0.));
#7682=DIRECTION('ref_axis',(1.,0.,0.));
#7683=DIRECTION('',(0.,1.,0.));
#7684=DIRECTION('center_axis',(0.,-1.,0.));
#7685=DIRECTION('ref_axis',(1.,0.,0.));
#7686=DIRECTION('center_axis',(0.866025403784439,0.,-0.5));
#7687=DIRECTION('ref_axis',(-0.5,0.,-0.866025403784439));
#7688=DIRECTION('',(0.866025403784439,0.,-0.5));
#7689=DIRECTION('center_axis',(0.866025403784439,0.,-0.5));
#7690=DIRECTION('ref_axis',(-0.5,0.,-0.866025403784439));
#7691=DIRECTION('',(0.866025403784439,0.,-0.5));
#7692=DIRECTION('center_axis',(0.,0.,1.));
#7693=DIRECTION('ref_axis',(1.,0.,0.));
#7694=DIRECTION('',(0.,0.,1.));
#7695=DIRECTION('center_axis',(0.,0.,1.));
#7696=DIRECTION('ref_axis',(1.,0.,0.));
#7697=DIRECTION('',(0.,0.,1.));
#7698=DIRECTION('center_axis',(0.,1.,0.));
#7699=DIRECTION('ref_axis',(0.,0.,1.));
#7700=DIRECTION('center_axis',(0.,-1.,0.));
#7701=DIRECTION('ref_axis',(1.,0.,0.));
#7702=DIRECTION('center_axis',(0.,1.,0.));
#7703=DIRECTION('ref_axis',(0.,0.,1.));
#7704=DIRECTION('center_axis',(0.,-1.,0.));
#7705=DIRECTION('ref_axis',(1.,0.,0.));
#7706=DIRECTION('center_axis',(0.,-1.,0.));
#7707=DIRECTION('ref_axis',(1.,0.,0.));
#7708=DIRECTION('center_axis',(0.,-1.,0.));
#7709=DIRECTION('ref_axis',(1.,0.,0.));
#7710=DIRECTION('',(0.,1.,0.));
#7711=DIRECTION('center_axis',(0.,-1.,0.));
#7712=DIRECTION('ref_axis',(0.,0.,-1.));
#7713=DIRECTION('center_axis',(0.,-1.,0.));
#7714=DIRECTION('ref_axis',(1.,0.,0.));
#7715=DIRECTION('center_axis',(0.,-1.,0.));
#7716=DIRECTION('ref_axis',(1.,0.,0.));
#7717=DIRECTION('',(0.,1.,0.));
#7718=DIRECTION('',(0.,0.,1.));
#7719=DIRECTION('',(1.,0.,0.));
#7720=DIRECTION('',(0.,0.,1.));
#7721=DIRECTION('',(1.,0.,0.));
#7722=DIRECTION('axis',(0.,0.,1.));
#7723=DIRECTION('refdir',(1.,0.,0.));
#7724=DIRECTION('center_axis',(0.,1.,0.));
#7725=DIRECTION('ref_axis',(0.,0.,1.));
#7726=DIRECTION('center_axis',(0.,-1.,0.));
#7727=DIRECTION('ref_axis',(1.,0.,0.));
#7728=DIRECTION('center_axis',(0.,-1.,0.));
#7729=DIRECTION('ref_axis',(1.,0.,0.));
#7730=DIRECTION('center_axis',(0.,-1.,0.));
#7731=DIRECTION('ref_axis',(1.,0.,0.));
#7732=DIRECTION('',(0.707106781186548,0.707106781186547,8.65956056235493E-17));
#7733=DIRECTION('center_axis',(0.,-1.,0.));
#7734=DIRECTION('ref_axis',(1.,0.,0.));
#7735=DIRECTION('center_axis',(0.,-1.,0.));
#7736=DIRECTION('ref_axis',(1.,0.,0.));
#7737=DIRECTION('',(0.,1.,0.));
#7738=DIRECTION('center_axis',(0.,1.,0.));
#7739=DIRECTION('ref_axis',(1.,0.,0.));
#7740=DIRECTION('center_axis',(0.,-1.,0.));
#7741=DIRECTION('ref_axis',(1.,0.,0.));
#7742=DIRECTION('',(-0.707106781186548,0.707106781186547,-8.65956056235494E-17));
#7743=DIRECTION('center_axis',(0.,-1.,0.));
#7744=DIRECTION('ref_axis',(0.,0.,-1.));
#7745=DIRECTION('center_axis',(0.,-1.,0.));
#7746=DIRECTION('ref_axis',(1.,0.,0.));
#7747=DIRECTION('center_axis',(0.,1.,0.));
#7748=DIRECTION('ref_axis',(1.,0.,0.));
#7749=DIRECTION('center_axis',(0.,1.,0.));
#7750=DIRECTION('ref_axis',(1.,0.,0.));
#7751=DIRECTION('',(-0.447213595499958,0.894427190999916,-5.47678698264203E-17));
#7752=DIRECTION('center_axis',(0.,-1.,0.));
#7753=DIRECTION('ref_axis',(1.,0.,0.));
#7754=DIRECTION('center_axis',(0.,1.,0.));
#7755=DIRECTION('ref_axis',(1.,0.,0.));
#7756=DIRECTION('',(0.,1.,0.));
#7757=DIRECTION('center_axis',(0.,1.,0.));
#7758=DIRECTION('ref_axis',(1.,0.,0.));
#7759=DIRECTION('center_axis',(0.,-1.,0.));
#7760=DIRECTION('ref_axis',(1.,0.,0.));
#7761=DIRECTION('',(-0.707106781186547,0.707106781186548,-8.65956056235493E-17));
#7762=DIRECTION('center_axis',(0.,-1.,0.));
#7763=DIRECTION('ref_axis',(0.,0.,-1.));
#7764=DIRECTION('center_axis',(0.866025403784439,0.,-0.5));
#7765=DIRECTION('ref_axis',(0.5,0.,0.866025403784439));
#7766=DIRECTION('',(-0.5,0.,-0.866025403784439));
#7767=DIRECTION('',(0.,-1.,0.));
#7768=DIRECTION('',(0.5,0.,0.866025403784439));
#7769=DIRECTION('',(0.,-1.,0.));
#7770=DIRECTION('center_axis',(1.60246890531964E-16,0.,-1.));
#7771=DIRECTION('ref_axis',(1.,0.,1.60246890531964E-16));
#7772=DIRECTION('',(-1.,0.,-1.60246890531964E-16));
#7773=DIRECTION('',(0.,-1.,0.));
#7774=DIRECTION('',(1.,0.,1.60246890531964E-16));
#7775=DIRECTION('center_axis',(-0.866025403784439,0.,-0.5));
#7776=DIRECTION('ref_axis',(0.5,0.,-0.866025403784439));
#7777=DIRECTION('',(-0.5,0.,0.866025403784439));
#7778=DIRECTION('',(0.,-1.,0.));
#7779=DIRECTION('',(0.5,0.,-0.866025403784439));
#7780=DIRECTION('center_axis',(-0.866025403784439,0.,0.5));
#7781=DIRECTION('ref_axis',(-0.5,0.,-0.866025403784439));
#7782=DIRECTION('',(0.5,0.,0.866025403784439));
#7783=DIRECTION('',(0.,-1.,0.));
#7784=DIRECTION('',(-0.5,0.,-0.866025403784439));
#7785=DIRECTION('center_axis',(-1.60246890531964E-16,0.,1.));
#7786=DIRECTION('ref_axis',(-1.,0.,-1.60246890531964E-16));
#7787=DIRECTION('',(1.,0.,1.60246890531964E-16));
#7788=DIRECTION('',(0.,-1.,0.));
#7789=DIRECTION('',(-1.,0.,-1.60246890531964E-16));
#7790=DIRECTION('center_axis',(0.866025403784439,0.,0.5));
#7791=DIRECTION('ref_axis',(-0.5,0.,0.866025403784439));
#7792=DIRECTION('',(0.5,0.,-0.866025403784439));
#7793=DIRECTION('',(-0.5,0.,0.866025403784439));
#7794=DIRECTION('center_axis',(0.,1.,0.));
#7795=DIRECTION('ref_axis',(1.,0.,0.));
#7796=DIRECTION('center_axis',(0.,-1.,0.));
#7797=DIRECTION('ref_axis',(0.,0.,-1.));
#7798=DIRECTION('axis',(0.,0.,1.));
#7799=DIRECTION('refdir',(1.,0.,0.));
#7800=DIRECTION('axis',(0.,0.,1.));
#7801=DIRECTION('refdir',(1.,0.,0.));
#7802=DIRECTION('center_axis',(-1.,0.,0.));
#7803=DIRECTION('ref_axis',(0.,0.,1.));
#7804=DIRECTION('',(0.,-1.,0.));
#7805=DIRECTION('',(0.,0.,1.));
#7806=DIRECTION('',(0.,1.,0.));
#7807=DIRECTION('',(0.,0.,-1.));
#7808=DIRECTION('center_axis',(0.,1.,0.));
#7809=DIRECTION('ref_axis',(1.,0.,0.));
#7810=DIRECTION('center_axis',(0.,-1.,0.));
#7811=DIRECTION('ref_axis',(1.,0.,0.));
#7812=DIRECTION('',(-1.,0.,0.));
#7813=DIRECTION('',(0.,0.,1.));
#7814=DIRECTION('center_axis',(1.,0.,0.));
#7815=DIRECTION('ref_axis',(0.,0.,-1.));
#7816=DIRECTION('',(0.,1.,0.));
#7817=DIRECTION('',(0.,1.,0.));
#7818=DIRECTION('',(0.,0.,-1.));
#7819=DIRECTION('center_axis',(0.,0.,1.));
#7820=DIRECTION('ref_axis',(1.,0.,0.));
#7821=DIRECTION('',(1.,0.,0.));
#7822=DIRECTION('center_axis',(0.,1.,0.));
#7823=DIRECTION('ref_axis',(0.,0.,1.));
#7824=DIRECTION('center_axis',(0.,1.,0.));
#7825=DIRECTION('ref_axis',(1.,0.,0.));
#7826=DIRECTION('center_axis',(0.,1.,0.));
#7827=DIRECTION('ref_axis',(1.,0.,0.));
#7828=DIRECTION('center_axis',(0.,1.,0.));
#7829=DIRECTION('ref_axis',(1.,0.,0.));
#7830=DIRECTION('',(0.,1.,0.));
#7831=DIRECTION('center_axis',(0.,1.,0.));
#7832=DIRECTION('ref_axis',(1.,0.,0.));
#7833=DIRECTION('center_axis',(0.,1.,0.));
#7834=DIRECTION('ref_axis',(1.,0.,0.));
#7835=DIRECTION('center_axis',(-1.,0.,0.));
#7836=DIRECTION('ref_axis',(0.,0.,1.));
#7837=DIRECTION('',(0.,-1.,0.));
#7838=DIRECTION('',(0.,0.,1.));
#7839=DIRECTION('',(0.,1.,0.));
#7840=DIRECTION('',(0.,0.,-1.));
#7841=DIRECTION('center_axis',(0.,1.,0.));
#7842=DIRECTION('ref_axis',(1.,0.,0.));
#7843=DIRECTION('center_axis',(0.,-1.,0.));
#7844=DIRECTION('ref_axis',(1.,0.,0.));
#7845=DIRECTION('',(-1.,0.,0.));
#7846=DIRECTION('',(0.,0.,1.));
#7847=DIRECTION('center_axis',(1.,0.,0.));
#7848=DIRECTION('ref_axis',(0.,0.,-1.));
#7849=DIRECTION('',(0.,1.,0.));
#7850=DIRECTION('',(0.,1.,0.));
#7851=DIRECTION('',(0.,0.,-1.));
#7852=DIRECTION('center_axis',(0.,0.,1.));
#7853=DIRECTION('ref_axis',(1.,0.,0.));
#7854=DIRECTION('',(1.,0.,0.));
#7855=DIRECTION('center_axis',(0.,1.,0.));
#7856=DIRECTION('ref_axis',(0.,0.,1.));
#7857=DIRECTION('center_axis',(0.,1.,0.));
#7858=DIRECTION('ref_axis',(1.,0.,0.));
#7859=DIRECTION('center_axis',(0.,1.,0.));
#7860=DIRECTION('ref_axis',(1.,0.,0.));
#7861=DIRECTION('center_axis',(0.,1.,0.));
#7862=DIRECTION('ref_axis',(1.,0.,0.));
#7863=DIRECTION('',(0.,-1.,0.));
#7864=DIRECTION('center_axis',(0.,-1.,0.));
#7865=DIRECTION('ref_axis',(1.,0.,0.));
#7866=DIRECTION('center_axis',(0.,1.,0.));
#7867=DIRECTION('ref_axis',(1.,0.,0.));
#7868=DIRECTION('center_axis',(0.,1.,0.));
#7869=DIRECTION('ref_axis',(1.,0.,0.));
#7870=DIRECTION('center_axis',(0.,1.,0.));
#7871=DIRECTION('ref_axis',(1.,0.,0.));
#7872=DIRECTION('',(0.,-1.,0.));
#7873=DIRECTION('center_axis',(0.,1.,0.));
#7874=DIRECTION('ref_axis',(1.,0.,0.));
#7875=DIRECTION('center_axis',(0.,1.,0.));
#7876=DIRECTION('ref_axis',(1.,0.,0.));
#7877=DIRECTION('center_axis',(0.,1.,0.));
#7878=DIRECTION('ref_axis',(1.,0.,0.));
#7879=DIRECTION('center_axis',(0.,1.,0.));
#7880=DIRECTION('ref_axis',(1.,0.,0.));
#7881=DIRECTION('',(0.,-1.,0.));
#7882=DIRECTION('center_axis',(0.,1.,0.));
#7883=DIRECTION('ref_axis',(1.,0.,0.));
#7884=DIRECTION('center_axis',(0.,1.,0.));
#7885=DIRECTION('ref_axis',(1.,0.,0.));
#7886=DIRECTION('center_axis',(0.,1.,0.));
#7887=DIRECTION('ref_axis',(1.,0.,0.));
#7888=DIRECTION('axis',(0.,0.,1.));
#7889=DIRECTION('refdir',(1.,0.,0.));
#7890=DIRECTION('center_axis',(0.,1.,0.));
#7891=DIRECTION('ref_axis',(1.,0.,0.));
#7892=DIRECTION('center_axis',(0.,-1.,0.));
#7893=DIRECTION('ref_axis',(1.,0.,0.));
#7894=DIRECTION('',(0.,-1.,0.));
#7895=DIRECTION('center_axis',(0.,-1.,0.));
#7896=DIRECTION('ref_axis',(1.,0.,0.));
#7897=DIRECTION('center_axis',(0.,1.,0.));
#7898=DIRECTION('ref_axis',(1.,0.,0.));
#7899=DIRECTION('center_axis',(0.,1.,0.));
#7900=DIRECTION('ref_axis',(1.,0.,0.));
#7901=DIRECTION('',(0.,-1.,0.));
#7902=DIRECTION('center_axis',(0.,1.,0.));
#7903=DIRECTION('ref_axis',(1.,0.,0.));
#7904=DIRECTION('center_axis',(0.,1.,0.));
#7905=DIRECTION('ref_axis',(1.,0.,0.));
#7906=DIRECTION('center_axis',(0.,1.,0.));
#7907=DIRECTION('ref_axis',(1.,0.,0.));
#7908=DIRECTION('axis',(0.,0.,1.));
#7909=DIRECTION('refdir',(1.,0.,0.));
#7910=DIRECTION('center_axis',(0.,1.,0.));
#7911=DIRECTION('ref_axis',(1.,0.,0.));
#7912=DIRECTION('center_axis',(0.,-1.,0.));
#7913=DIRECTION('ref_axis',(1.,0.,0.));
#7914=DIRECTION('',(0.,-1.,0.));
#7915=DIRECTION('center_axis',(0.,-1.,0.));
#7916=DIRECTION('ref_axis',(1.,0.,0.));
#7917=DIRECTION('center_axis',(0.,1.,0.));
#7918=DIRECTION('ref_axis',(1.,0.,0.));
#7919=DIRECTION('center_axis',(0.,1.,0.));
#7920=DIRECTION('ref_axis',(1.,0.,0.));
#7921=DIRECTION('',(0.,-1.,0.));
#7922=DIRECTION('center_axis',(0.,1.,0.));
#7923=DIRECTION('ref_axis',(1.,0.,0.));
#7924=DIRECTION('center_axis',(0.,1.,0.));
#7925=DIRECTION('ref_axis',(1.,0.,0.));
#7926=DIRECTION('center_axis',(0.,1.,0.));
#7927=DIRECTION('ref_axis',(1.,0.,0.));
#7928=DIRECTION('axis',(0.,0.,1.));
#7929=DIRECTION('refdir',(1.,0.,0.));
#7930=DIRECTION('center_axis',(0.,1.,0.));
#7931=DIRECTION('ref_axis',(1.,0.,0.));
#7932=DIRECTION('center_axis',(0.,-1.,0.));
#7933=DIRECTION('ref_axis',(1.,0.,0.));
#7934=DIRECTION('',(0.,-1.,0.));
#7935=DIRECTION('center_axis',(0.,-1.,0.));
#7936=DIRECTION('ref_axis',(1.,0.,0.));
#7937=DIRECTION('center_axis',(0.,1.,0.));
#7938=DIRECTION('ref_axis',(1.,0.,0.));
#7939=DIRECTION('center_axis',(0.,1.,0.));
#7940=DIRECTION('ref_axis',(1.,0.,0.));
#7941=DIRECTION('',(0.,-1.,0.));
#7942=DIRECTION('center_axis',(0.,1.,0.));
#7943=DIRECTION('ref_axis',(1.,0.,0.));
#7944=DIRECTION('center_axis',(0.,1.,0.));
#7945=DIRECTION('ref_axis',(1.,0.,0.));
#7946=DIRECTION('center_axis',(0.,1.,0.));
#7947=DIRECTION('ref_axis',(1.,0.,0.));
#7948=DIRECTION('axis',(0.,0.,1.));
#7949=DIRECTION('refdir',(1.,0.,0.));
#7950=DIRECTION('center_axis',(0.,0.,1.));
#7951=DIRECTION('ref_axis',(1.,0.,0.));
#7952=DIRECTION('',(0.,1.,0.));
#7953=DIRECTION('center_axis',(0.,0.,1.));
#7954=DIRECTION('ref_axis',(1.,0.,0.));
#7955=DIRECTION('center_axis',(0.,0.,1.));
#7956=DIRECTION('ref_axis',(1.,0.,0.));
#7957=DIRECTION('center_axis',(0.,0.,1.));
#7958=DIRECTION('ref_axis',(1.,0.,0.));
#7959=DIRECTION('',(0.,0.,1.));
#7960=DIRECTION('center_axis',(0.,0.,1.));
#7961=DIRECTION('ref_axis',(1.,0.,0.));
#7962=DIRECTION('center_axis',(0.,0.,1.));
#7963=DIRECTION('ref_axis',(1.,0.,0.));
#7964=DIRECTION('',(0.,-1.,0.));
#7965=DIRECTION('center_axis',(0.,1.,0.));
#7966=DIRECTION('ref_axis',(1.,0.,0.));
#7967=DIRECTION('center_axis',(0.,-1.,0.));
#7968=DIRECTION('ref_axis',(1.,0.,0.));
#7969=DIRECTION('',(0.,-1.,0.));
#7970=DIRECTION('center_axis',(0.,-1.,0.));
#7971=DIRECTION('ref_axis',(1.,0.,0.));
#7972=DIRECTION('center_axis',(0.,1.,0.));
#7973=DIRECTION('ref_axis',(1.,0.,0.));
#7974=DIRECTION('center_axis',(0.,1.,0.));
#7975=DIRECTION('ref_axis',(1.,0.,0.));
#7976=DIRECTION('',(0.,-1.,0.));
#7977=DIRECTION('center_axis',(0.,1.,0.));
#7978=DIRECTION('ref_axis',(1.,0.,0.));
#7979=DIRECTION('center_axis',(0.,1.,0.));
#7980=DIRECTION('ref_axis',(1.,0.,0.));
#7981=DIRECTION('center_axis',(0.,1.,0.));
#7982=DIRECTION('ref_axis',(1.,0.,0.));
#7983=DIRECTION('axis',(0.,0.,1.));
#7984=DIRECTION('refdir',(1.,0.,0.));
#7985=DIRECTION('center_axis',(0.,0.,1.));
#7986=DIRECTION('ref_axis',(1.,0.,0.));
#7987=DIRECTION('',(0.,1.,0.));
#7988=DIRECTION('center_axis',(0.,0.,1.));
#7989=DIRECTION('ref_axis',(1.,0.,0.));
#7990=DIRECTION('center_axis',(0.,0.,1.));
#7991=DIRECTION('ref_axis',(1.,0.,0.));
#7992=DIRECTION('center_axis',(0.,0.,1.));
#7993=DIRECTION('ref_axis',(1.,0.,0.));
#7994=DIRECTION('',(0.,0.,1.));
#7995=DIRECTION('center_axis',(0.,0.,1.));
#7996=DIRECTION('ref_axis',(1.,0.,0.));
#7997=DIRECTION('center_axis',(0.,0.,1.));
#7998=DIRECTION('ref_axis',(1.,0.,0.));
#7999=DIRECTION('',(0.,-1.,0.));
#8000=DIRECTION('center_axis',(0.,1.,0.));
#8001=DIRECTION('ref_axis',(1.,0.,0.));
#8002=DIRECTION('center_axis',(0.,-1.,0.));
#8003=DIRECTION('ref_axis',(1.,0.,0.));
#8004=DIRECTION('',(0.,-1.,0.));
#8005=DIRECTION('center_axis',(0.,-1.,0.));
#8006=DIRECTION('ref_axis',(1.,0.,0.));
#8007=DIRECTION('center_axis',(0.,1.,0.));
#8008=DIRECTION('ref_axis',(1.,0.,0.));
#8009=DIRECTION('center_axis',(0.,1.,0.));
#8010=DIRECTION('ref_axis',(1.,0.,0.));
#8011=DIRECTION('',(0.,-1.,0.));
#8012=DIRECTION('center_axis',(0.,1.,0.));
#8013=DIRECTION('ref_axis',(1.,0.,0.));
#8014=DIRECTION('center_axis',(0.,1.,0.));
#8015=DIRECTION('ref_axis',(1.,0.,0.));
#8016=DIRECTION('center_axis',(0.,1.,0.));
#8017=DIRECTION('ref_axis',(1.,0.,0.));
#8018=DIRECTION('axis',(0.,0.,1.));
#8019=DIRECTION('refdir',(1.,0.,0.));
#8020=DIRECTION('center_axis',(-1.,0.,0.));
#8021=DIRECTION('ref_axis',(0.,0.,1.));
#8022=DIRECTION('',(0.,0.,1.));
#8023=DIRECTION('',(0.,1.,0.));
#8024=DIRECTION('',(0.,0.,-1.));
#8025=DIRECTION('',(0.,1.,0.));
#8026=DIRECTION('center_axis',(0.,0.,-1.));
#8027=DIRECTION('ref_axis',(-1.,0.,0.));
#8028=DIRECTION('',(-1.,0.,0.));
#8029=DIRECTION('',(0.,1.,0.));
#8030=DIRECTION('',(1.,0.,0.));
#8031=DIRECTION('center_axis',(1.,0.,0.));
#8032=DIRECTION('ref_axis',(0.,0.,-1.));
#8033=DIRECTION('',(0.,0.,-1.));
#8034=DIRECTION('',(0.,-1.,0.));
#8035=DIRECTION('',(0.,0.,1.));
#8036=DIRECTION('center_axis',(0.,1.,0.));
#8037=DIRECTION('ref_axis',(1.,0.,0.));
#8038=DIRECTION('center_axis',(0.,1.,0.));
#8039=DIRECTION('ref_axis',(1.,0.,0.));
#8040=DIRECTION('center_axis',(0.,-1.,0.));
#8041=DIRECTION('ref_axis',(1.,0.,0.));
#8042=DIRECTION('center_axis',(0.,-1.,0.));
#8043=DIRECTION('ref_axis',(1.,0.,0.));
#8044=DIRECTION('center_axis',(0.,-1.,0.));
#8045=DIRECTION('ref_axis',(1.,0.,0.));
#8046=DIRECTION('center_axis',(0.,-1.,0.));
#8047=DIRECTION('ref_axis',(1.,0.,0.));
#8048=DIRECTION('center_axis',(0.,-1.,0.));
#8049=DIRECTION('ref_axis',(1.,0.,0.));
#8050=DIRECTION('center_axis',(0.,-1.,0.));
#8051=DIRECTION('ref_axis',(1.,0.,0.));
#8052=DIRECTION('center_axis',(0.,-1.,0.));
#8053=DIRECTION('ref_axis',(1.,0.,0.));
#8054=DIRECTION('center_axis',(0.,1.,0.));
#8055=DIRECTION('ref_axis',(-1.83697019872103E-16,0.,1.));
#8056=DIRECTION('center_axis',(0.,-1.,0.));
#8057=DIRECTION('ref_axis',(1.,0.,0.));
#8058=DIRECTION('center_axis',(0.,1.,0.));
#8059=DIRECTION('ref_axis',(1.,0.,0.));
#8060=DIRECTION('center_axis',(0.,1.,0.));
#8061=DIRECTION('ref_axis',(1.,0.,0.));
#8062=DIRECTION('',(0.,1.,0.));
#8063=DIRECTION('center_axis',(0.,1.,0.));
#8064=DIRECTION('ref_axis',(1.,0.,0.));
#8065=DIRECTION('center_axis',(0.,1.,0.));
#8066=DIRECTION('ref_axis',(1.,0.,0.));
#8067=DIRECTION('',(0.,1.,0.));
#8068=DIRECTION('center_axis',(0.,1.,0.));
#8069=DIRECTION('ref_axis',(1.,0.,0.));
#8070=DIRECTION('center_axis',(0.,1.,0.));
#8071=DIRECTION('ref_axis',(1.,0.,0.));
#8072=DIRECTION('',(0.,1.,0.));
#8073=DIRECTION('center_axis',(0.,1.,0.));
#8074=DIRECTION('ref_axis',(1.,0.,0.));
#8075=DIRECTION('center_axis',(0.,1.,0.));
#8076=DIRECTION('ref_axis',(1.,0.,0.));
#8077=DIRECTION('',(0.,1.,0.));
#8078=DIRECTION('center_axis',(0.,1.,0.));
#8079=DIRECTION('ref_axis',(1.,0.,0.));
#8080=DIRECTION('center_axis',(0.,1.,0.));
#8081=DIRECTION('ref_axis',(1.,0.,0.));
#8082=DIRECTION('',(0.,1.,0.));
#8083=DIRECTION('center_axis',(0.,1.,0.));
#8084=DIRECTION('ref_axis',(1.,0.,0.));
#8085=DIRECTION('center_axis',(0.,1.,0.));
#8086=DIRECTION('ref_axis',(1.,0.,0.));
#8087=DIRECTION('',(0.,1.,0.));
#8088=DIRECTION('center_axis',(0.,1.,0.));
#8089=DIRECTION('ref_axis',(1.,0.,0.));
#8090=DIRECTION('center_axis',(0.,1.,0.));
#8091=DIRECTION('ref_axis',(1.,0.,0.));
#8092=DIRECTION('center_axis',(0.,-1.,0.));
#8093=DIRECTION('ref_axis',(1.,0.,0.));
#8094=DIRECTION('center_axis',(0.,1.,0.));
#8095=DIRECTION('ref_axis',(1.,0.,0.));
#8096=DIRECTION('',(0.,-1.,0.));
#8097=DIRECTION('center_axis',(0.,1.,0.));
#8098=DIRECTION('ref_axis',(1.,0.,0.));
#8099=DIRECTION('',(0.,-1.,0.));
#8100=DIRECTION('center_axis',(0.,1.,0.));
#8101=DIRECTION('ref_axis',(1.,0.,0.));
#8102=DIRECTION('center_axis',(0.,1.,0.));
#8103=DIRECTION('ref_axis',(1.,0.,0.));
#8104=DIRECTION('axis',(0.,0.,1.));
#8105=DIRECTION('refdir',(1.,0.,0.));
#8106=DIRECTION('center_axis',(0.,1.,0.));
#8107=DIRECTION('ref_axis',(1.,0.,0.));
#8108=DIRECTION('center_axis',(0.,-1.,0.));
#8109=DIRECTION('ref_axis',(1.,0.,0.));
#8110=DIRECTION('',(0.,-1.,0.));
#8111=DIRECTION('center_axis',(0.,-1.,0.));
#8112=DIRECTION('ref_axis',(1.,0.,0.));
#8113=DIRECTION('center_axis',(0.,1.,0.));
#8114=DIRECTION('ref_axis',(1.,0.,0.));
#8115=DIRECTION('center_axis',(0.,1.,0.));
#8116=DIRECTION('ref_axis',(1.,0.,0.));
#8117=DIRECTION('',(0.,-1.,0.));
#8118=DIRECTION('center_axis',(0.,1.,0.));
#8119=DIRECTION('ref_axis',(1.,0.,0.));
#8120=DIRECTION('center_axis',(0.,1.,0.));
#8121=DIRECTION('ref_axis',(1.,0.,0.));
#8122=DIRECTION('center_axis',(0.,1.,0.));
#8123=DIRECTION('ref_axis',(1.,0.,0.));
#8124=DIRECTION('axis',(0.,0.,1.));
#8125=DIRECTION('refdir',(1.,0.,0.));
#8126=DIRECTION('center_axis',(-1.,0.,0.));
#8127=DIRECTION('ref_axis',(0.,0.,1.));
#8128=DIRECTION('',(0.,0.,1.));
#8129=DIRECTION('',(0.,1.,0.));
#8130=DIRECTION('',(0.,0.,-1.));
#8131=DIRECTION('',(0.,1.,0.));
#8132=DIRECTION('center_axis',(0.,0.,-1.));
#8133=DIRECTION('ref_axis',(-1.,0.,0.));
#8134=DIRECTION('',(-1.,0.,0.));
#8135=DIRECTION('',(0.,1.,0.));
#8136=DIRECTION('',(1.,0.,0.));
#8137=DIRECTION('center_axis',(0.,0.,1.));
#8138=DIRECTION('ref_axis',(1.,0.,0.));
#8139=DIRECTION('center_axis',(1.,0.,0.));
#8140=DIRECTION('ref_axis',(0.,0.,-1.));
#8141=DIRECTION('',(0.,0.,-1.));
#8142=DIRECTION('',(0.,-1.,0.));
#8143=DIRECTION('',(0.,0.,1.));
#8144=DIRECTION('center_axis',(0.,1.,0.));
#8145=DIRECTION('ref_axis',(1.,0.,0.));
#8146=DIRECTION('center_axis',(0.,1.,0.));
#8147=DIRECTION('ref_axis',(1.,0.,0.));
#8148=DIRECTION('center_axis',(0.,-1.,0.));
#8149=DIRECTION('ref_axis',(1.,0.,0.));
#8150=DIRECTION('center_axis',(0.,1.,0.));
#8151=DIRECTION('ref_axis',(-1.83697019872103E-16,0.,1.));
#8152=DIRECTION('center_axis',(0.,1.,0.));
#8153=DIRECTION('ref_axis',(1.,0.,0.));
#8154=DIRECTION('center_axis',(1.,0.,6.12323399573677E-17));
#8155=DIRECTION('ref_axis',(6.12323399573677E-17,0.,-1.));
#8156=DIRECTION('',(1.,0.,6.12323399573677E-17));
#8157=DIRECTION('center_axis',(1.,0.,6.12323399573677E-17));
#8158=DIRECTION('ref_axis',(6.12323399573677E-17,0.,-1.));
#8159=DIRECTION('',(1.,0.,6.12323399573677E-17));
#8160=DIRECTION('center_axis',(0.,-1.,0.));
#8161=DIRECTION('ref_axis',(1.,0.,0.));
#8162=DIRECTION('center_axis',(0.,-1.,0.));
#8163=DIRECTION('ref_axis',(1.,0.,0.));
#8164=DIRECTION('',(0.,1.,0.));
#8165=DIRECTION('',(0.,1.,0.));
#8166=DIRECTION('center_axis',(0.,1.,0.));
#8167=DIRECTION('ref_axis',(1.,0.,0.));
#8168=DIRECTION('center_axis',(0.,0.,1.));
#8169=DIRECTION('ref_axis',(1.,0.,0.));
#8170=DIRECTION('',(0.,0.,1.));
#8171=DIRECTION('center_axis',(0.,0.,1.));
#8172=DIRECTION('ref_axis',(1.,0.,0.));
#8173=DIRECTION('',(0.,0.,1.));
#8174=DIRECTION('center_axis',(0.,1.,0.));
#8175=DIRECTION('ref_axis',(1.,0.,0.));
#8176=DIRECTION('center_axis',(0.,1.,0.));
#8177=DIRECTION('ref_axis',(1.,0.,0.));
#8178=DIRECTION('center_axis',(0.,1.,0.));
#8179=DIRECTION('ref_axis',(1.,0.,0.));
#8180=DIRECTION('center_axis',(0.,1.,0.));
#8181=DIRECTION('ref_axis',(0.987688340595138,0.,0.156434465040231));
#8182=DIRECTION('center_axis',(0.,1.,0.));
#8183=DIRECTION('ref_axis',(1.,0.,0.));
#8184=DIRECTION('center_axis',(0.,1.,0.));
#8185=DIRECTION('ref_axis',(0.951056516295154,0.,0.309016994374948));
#8186=DIRECTION('center_axis',(0.,1.,0.));
#8187=DIRECTION('ref_axis',(1.,0.,0.));
#8188=DIRECTION('center_axis',(0.,1.,0.));
#8189=DIRECTION('ref_axis',(0.891006524188368,0.,0.453990499739547));
#8190=DIRECTION('center_axis',(0.,1.,0.));
#8191=DIRECTION('ref_axis',(1.,0.,0.));
#8192=DIRECTION('center_axis',(0.,1.,0.));
#8193=DIRECTION('ref_axis',(0.809016994374947,0.,0.587785252292473));
#8194=DIRECTION('center_axis',(0.,1.,0.));
#8195=DIRECTION('ref_axis',(1.,0.,0.));
#8196=DIRECTION('center_axis',(0.,1.,0.));
#8197=DIRECTION('ref_axis',(0.707106781186547,0.,0.707106781186548));
#8198=DIRECTION('center_axis',(0.,1.,0.));
#8199=DIRECTION('ref_axis',(1.,0.,0.));
#8200=DIRECTION('center_axis',(0.,1.,0.));
#8201=DIRECTION('ref_axis',(0.587785252292473,0.,0.809016994374948));
#8202=DIRECTION('center_axis',(0.,1.,0.));
#8203=DIRECTION('ref_axis',(1.,0.,0.));
#8204=DIRECTION('center_axis',(0.,1.,0.));
#8205=DIRECTION('ref_axis',(0.453990499739547,0.,0.891006524188368));
#8206=DIRECTION('center_axis',(0.,1.,0.));
#8207=DIRECTION('ref_axis',(1.,0.,0.));
#8208=DIRECTION('center_axis',(0.,1.,0.));
#8209=DIRECTION('ref_axis',(0.309016994374947,0.,0.951056516295154));
#8210=DIRECTION('center_axis',(0.,1.,0.));
#8211=DIRECTION('ref_axis',(1.,0.,0.));
#8212=DIRECTION('center_axis',(0.,1.,0.));
#8213=DIRECTION('ref_axis',(0.156434465040231,0.,0.987688340595138));
#8214=DIRECTION('center_axis',(0.,1.,0.));
#8215=DIRECTION('ref_axis',(1.,0.,0.));
#8216=DIRECTION('center_axis',(0.,1.,0.));
#8217=DIRECTION('ref_axis',(-1.83697019872103E-16,0.,1.));
#8218=DIRECTION('center_axis',(0.,1.,0.));
#8219=DIRECTION('ref_axis',(1.,0.,0.));
#8220=DIRECTION('center_axis',(0.,1.,0.));
#8221=DIRECTION('ref_axis',(-0.156434465040231,0.,0.987688340595138));
#8222=DIRECTION('center_axis',(0.,1.,0.));
#8223=DIRECTION('ref_axis',(1.,0.,0.));
#8224=DIRECTION('center_axis',(0.,1.,0.));
#8225=DIRECTION('ref_axis',(-0.309016994374948,0.,0.951056516295154));
#8226=DIRECTION('center_axis',(0.,1.,0.));
#8227=DIRECTION('ref_axis',(1.,0.,0.));
#8228=DIRECTION('center_axis',(0.,1.,0.));
#8229=DIRECTION('ref_axis',(-0.453990499739547,0.,0.891006524188368));
#8230=DIRECTION('center_axis',(0.,1.,0.));
#8231=DIRECTION('ref_axis',(1.,0.,0.));
#8232=DIRECTION('center_axis',(0.,1.,0.));
#8233=DIRECTION('ref_axis',(-0.587785252292473,0.,0.809016994374947));
#8234=DIRECTION('center_axis',(0.,1.,0.));
#8235=DIRECTION('ref_axis',(1.,0.,0.));
#8236=DIRECTION('center_axis',(0.,1.,0.));
#8237=DIRECTION('ref_axis',(-0.707106781186548,0.,0.707106781186547));
#8238=DIRECTION('center_axis',(0.,1.,0.));
#8239=DIRECTION('ref_axis',(1.,0.,0.));
#8240=DIRECTION('center_axis',(0.,1.,0.));
#8241=DIRECTION('ref_axis',(-0.809016994374947,0.,0.587785252292473));
#8242=DIRECTION('center_axis',(0.,1.,0.));
#8243=DIRECTION('ref_axis',(1.,0.,0.));
#8244=DIRECTION('center_axis',(0.,1.,0.));
#8245=DIRECTION('ref_axis',(-0.891006524188368,0.,0.453990499739547));
#8246=DIRECTION('center_axis',(0.,1.,0.));
#8247=DIRECTION('ref_axis',(1.,0.,0.));
#8248=DIRECTION('center_axis',(0.,1.,0.));
#8249=DIRECTION('ref_axis',(-0.951056516295154,0.,0.309016994374947));
#8250=DIRECTION('center_axis',(0.,1.,0.));
#8251=DIRECTION('ref_axis',(1.,0.,0.));
#8252=DIRECTION('center_axis',(0.,1.,0.));
#8253=DIRECTION('ref_axis',(-0.987688340595138,0.,0.156434465040231));
#8254=DIRECTION('center_axis',(0.,1.,0.));
#8255=DIRECTION('ref_axis',(1.,0.,0.));
#8256=DIRECTION('center_axis',(0.,1.,0.));
#8257=DIRECTION('ref_axis',(-1.,0.,-1.22464679914735E-16));
#8258=DIRECTION('center_axis',(0.,1.,0.));
#8259=DIRECTION('ref_axis',(1.,0.,0.));
#8260=DIRECTION('center_axis',(0.,1.,0.));
#8261=DIRECTION('ref_axis',(-0.987688340595138,0.,-0.156434465040231));
#8262=DIRECTION('center_axis',(0.,1.,0.));
#8263=DIRECTION('ref_axis',(1.,0.,0.));
#8264=DIRECTION('center_axis',(0.,1.,0.));
#8265=DIRECTION('ref_axis',(-0.951056516295154,0.,-0.309016994374948));
#8266=DIRECTION('center_axis',(0.,1.,0.));
#8267=DIRECTION('ref_axis',(1.,0.,0.));
#8268=DIRECTION('center_axis',(0.,1.,0.));
#8269=DIRECTION('ref_axis',(-0.891006524188368,0.,-0.453990499739547));
#8270=DIRECTION('center_axis',(0.,1.,0.));
#8271=DIRECTION('ref_axis',(1.,0.,0.));
#8272=DIRECTION('center_axis',(0.,1.,0.));
#8273=DIRECTION('ref_axis',(-0.809016994374947,0.,-0.587785252292473));
#8274=DIRECTION('center_axis',(0.,1.,0.));
#8275=DIRECTION('ref_axis',(1.,0.,0.));
#8276=DIRECTION('center_axis',(0.,1.,0.));
#8277=DIRECTION('ref_axis',(-0.707106781186547,0.,-0.707106781186548));
#8278=DIRECTION('center_axis',(0.,1.,0.));
#8279=DIRECTION('ref_axis',(1.,0.,0.));
#8280=DIRECTION('center_axis',(0.,1.,0.));
#8281=DIRECTION('ref_axis',(-0.587785252292473,0.,-0.809016994374947));
#8282=DIRECTION('center_axis',(0.,1.,0.));
#8283=DIRECTION('ref_axis',(1.,0.,0.));
#8284=DIRECTION('center_axis',(0.,1.,0.));
#8285=DIRECTION('ref_axis',(-0.453990499739547,0.,-0.891006524188368));
#8286=DIRECTION('center_axis',(0.,1.,0.));
#8287=DIRECTION('ref_axis',(1.,0.,0.));
#8288=DIRECTION('center_axis',(0.,1.,0.));
#8289=DIRECTION('ref_axis',(-0.309016994374947,0.,-0.951056516295154));
#8290=DIRECTION('center_axis',(0.,1.,0.));
#8291=DIRECTION('ref_axis',(1.,0.,0.));
#8292=DIRECTION('center_axis',(0.,1.,0.));
#8293=DIRECTION('ref_axis',(-0.156434465040231,0.,-0.987688340595138));
#8294=DIRECTION('center_axis',(0.,1.,0.));
#8295=DIRECTION('ref_axis',(1.,0.,0.));
#8296=DIRECTION('center_axis',(0.,1.,0.));
#8297=DIRECTION('ref_axis',(6.12323399573677E-17,0.,-1.));
#8298=DIRECTION('center_axis',(0.,1.,0.));
#8299=DIRECTION('ref_axis',(1.,0.,0.));
#8300=DIRECTION('center_axis',(0.,1.,0.));
#8301=DIRECTION('ref_axis',(0.156434465040231,0.,-0.987688340595138));
#8302=DIRECTION('center_axis',(0.,1.,0.));
#8303=DIRECTION('ref_axis',(1.,0.,0.));
#8304=DIRECTION('center_axis',(0.,1.,0.));
#8305=DIRECTION('ref_axis',(0.309016994374948,0.,-0.951056516295154));
#8306=DIRECTION('center_axis',(0.,1.,0.));
#8307=DIRECTION('ref_axis',(1.,0.,0.));
#8308=DIRECTION('center_axis',(0.,1.,0.));
#8309=DIRECTION('ref_axis',(0.453990499739547,0.,-0.891006524188368));
#8310=DIRECTION('center_axis',(0.,1.,0.));
#8311=DIRECTION('ref_axis',(1.,0.,0.));
#8312=DIRECTION('center_axis',(0.,1.,0.));
#8313=DIRECTION('ref_axis',(0.587785252292473,0.,-0.809016994374947));
#8314=DIRECTION('center_axis',(0.,1.,0.));
#8315=DIRECTION('ref_axis',(1.,0.,0.));
#8316=DIRECTION('center_axis',(0.,1.,0.));
#8317=DIRECTION('ref_axis',(0.707106781186548,0.,-0.707106781186547));
#8318=DIRECTION('center_axis',(0.,1.,0.));
#8319=DIRECTION('ref_axis',(1.,0.,0.));
#8320=DIRECTION('center_axis',(0.,1.,0.));
#8321=DIRECTION('ref_axis',(0.809016994374947,0.,-0.587785252292473));
#8322=DIRECTION('center_axis',(0.,1.,0.));
#8323=DIRECTION('ref_axis',(1.,0.,0.));
#8324=DIRECTION('center_axis',(0.,1.,0.));
#8325=DIRECTION('ref_axis',(0.891006524188368,0.,-0.453990499739547));
#8326=DIRECTION('center_axis',(0.,1.,0.));
#8327=DIRECTION('ref_axis',(1.,0.,0.));
#8328=DIRECTION('center_axis',(0.,1.,0.));
#8329=DIRECTION('ref_axis',(0.951056516295154,0.,-0.309016994374947));
#8330=DIRECTION('center_axis',(0.,1.,0.));
#8331=DIRECTION('ref_axis',(1.,0.,0.));
#8332=DIRECTION('center_axis',(0.,1.,0.));
#8333=DIRECTION('ref_axis',(0.987688340595138,0.,-0.156434465040231));
#8334=DIRECTION('center_axis',(0.,1.,0.));
#8335=DIRECTION('ref_axis',(1.,0.,0.));
#8336=DIRECTION('center_axis',(0.,1.,0.));
#8337=DIRECTION('ref_axis',(1.,0.,0.));
#8338=DIRECTION('center_axis',(0.,1.,0.));
#8339=DIRECTION('ref_axis',(1.,0.,0.));
#8340=DIRECTION('center_axis',(0.,-1.,0.));
#8341=DIRECTION('ref_axis',(1.,0.,0.));
#8342=DIRECTION('center_axis',(0.,-1.,0.));
#8343=DIRECTION('ref_axis',(1.,0.,0.));
#8344=DIRECTION('',(0.,1.,0.));
#8345=DIRECTION('center_axis',(0.,1.,0.));
#8346=DIRECTION('ref_axis',(1.,0.,0.));
#8347=DIRECTION('center_axis',(0.,1.,0.));
#8348=DIRECTION('ref_axis',(1.,0.,0.));
#8349=DIRECTION('center_axis',(0.,1.,0.));
#8350=DIRECTION('ref_axis',(1.,0.,0.));
#8351=DIRECTION('center_axis',(0.,-1.,0.));
#8352=DIRECTION('ref_axis',(0.987688340595138,0.,0.156434465040231));
#8353=DIRECTION('center_axis',(0.,1.,0.));
#8354=DIRECTION('ref_axis',(1.,0.,0.));
#8355=DIRECTION('center_axis',(0.,-1.,0.));
#8356=DIRECTION('ref_axis',(1.,0.,0.));
#8357=DIRECTION('center_axis',(0.,1.,0.));
#8358=DIRECTION('ref_axis',(1.,0.,0.));
#8359=DIRECTION('center_axis',(0.,-1.,0.));
#8360=DIRECTION('ref_axis',(0.987688340595138,0.,-0.156434465040231));
#8361=DIRECTION('center_axis',(0.,1.,0.));
#8362=DIRECTION('ref_axis',(1.,0.,0.));
#8363=DIRECTION('center_axis',(0.,-1.,0.));
#8364=DIRECTION('ref_axis',(0.951056516295154,0.,-0.309016994374947));
#8365=DIRECTION('center_axis',(0.,1.,0.));
#8366=DIRECTION('ref_axis',(1.,0.,0.));
#8367=DIRECTION('center_axis',(0.,-1.,0.));
#8368=DIRECTION('ref_axis',(0.891006524188368,0.,-0.453990499739547));
#8369=DIRECTION('center_axis',(0.,1.,0.));
#8370=DIRECTION('ref_axis',(1.,0.,0.));
#8371=DIRECTION('center_axis',(0.,-1.,0.));
#8372=DIRECTION('ref_axis',(0.809016994374947,0.,-0.587785252292473));
#8373=DIRECTION('center_axis',(0.,1.,0.));
#8374=DIRECTION('ref_axis',(1.,0.,0.));
#8375=DIRECTION('center_axis',(0.,-1.,0.));
#8376=DIRECTION('ref_axis',(0.707106781186548,0.,-0.707106781186547));
#8377=DIRECTION('center_axis',(0.,1.,0.));
#8378=DIRECTION('ref_axis',(1.,0.,0.));
#8379=DIRECTION('center_axis',(0.,-1.,0.));
#8380=DIRECTION('ref_axis',(0.587785252292473,0.,-0.809016994374947));
#8381=DIRECTION('center_axis',(0.,1.,0.));
#8382=DIRECTION('ref_axis',(1.,0.,0.));
#8383=DIRECTION('center_axis',(0.,-1.,0.));
#8384=DIRECTION('ref_axis',(0.453990499739547,0.,-0.891006524188368));
#8385=DIRECTION('center_axis',(0.,1.,0.));
#8386=DIRECTION('ref_axis',(1.,0.,0.));
#8387=DIRECTION('center_axis',(0.,-1.,0.));
#8388=DIRECTION('ref_axis',(0.309016994374948,0.,-0.951056516295154));
#8389=DIRECTION('center_axis',(0.,1.,0.));
#8390=DIRECTION('ref_axis',(1.,0.,0.));
#8391=DIRECTION('center_axis',(0.,-1.,0.));
#8392=DIRECTION('ref_axis',(0.156434465040231,0.,-0.987688340595138));
#8393=DIRECTION('center_axis',(0.,1.,0.));
#8394=DIRECTION('ref_axis',(1.,0.,0.));
#8395=DIRECTION('center_axis',(0.,-1.,0.));
#8396=DIRECTION('ref_axis',(6.12323399573677E-17,0.,-1.));
#8397=DIRECTION('center_axis',(0.,1.,0.));
#8398=DIRECTION('ref_axis',(1.,0.,0.));
#8399=DIRECTION('center_axis',(0.,-1.,0.));
#8400=DIRECTION('ref_axis',(-0.156434465040231,0.,-0.987688340595138));
#8401=DIRECTION('center_axis',(0.,1.,0.));
#8402=DIRECTION('ref_axis',(1.,0.,0.));
#8403=DIRECTION('center_axis',(0.,-1.,0.));
#8404=DIRECTION('ref_axis',(-0.309016994374947,0.,-0.951056516295154));
#8405=DIRECTION('center_axis',(0.,1.,0.));
#8406=DIRECTION('ref_axis',(1.,0.,0.));
#8407=DIRECTION('center_axis',(0.,-1.,0.));
#8408=DIRECTION('ref_axis',(-0.453990499739547,0.,-0.891006524188368));
#8409=DIRECTION('center_axis',(0.,1.,0.));
#8410=DIRECTION('ref_axis',(1.,0.,0.));
#8411=DIRECTION('center_axis',(0.,-1.,0.));
#8412=DIRECTION('ref_axis',(-0.587785252292473,0.,-0.809016994374947));
#8413=DIRECTION('center_axis',(0.,1.,0.));
#8414=DIRECTION('ref_axis',(1.,0.,0.));
#8415=DIRECTION('center_axis',(0.,-1.,0.));
#8416=DIRECTION('ref_axis',(-0.707106781186547,0.,-0.707106781186548));
#8417=DIRECTION('center_axis',(0.,1.,0.));
#8418=DIRECTION('ref_axis',(1.,0.,0.));
#8419=DIRECTION('center_axis',(0.,-1.,0.));
#8420=DIRECTION('ref_axis',(-0.809016994374947,0.,-0.587785252292473));
#8421=DIRECTION('center_axis',(0.,1.,0.));
#8422=DIRECTION('ref_axis',(1.,0.,0.));
#8423=DIRECTION('center_axis',(0.,-1.,0.));
#8424=DIRECTION('ref_axis',(-0.891006524188368,0.,-0.453990499739547));
#8425=DIRECTION('center_axis',(0.,1.,0.));
#8426=DIRECTION('ref_axis',(1.,0.,0.));
#8427=DIRECTION('center_axis',(0.,-1.,0.));
#8428=DIRECTION('ref_axis',(-0.951056516295154,0.,-0.309016994374948));
#8429=DIRECTION('center_axis',(0.,1.,0.));
#8430=DIRECTION('ref_axis',(1.,0.,0.));
#8431=DIRECTION('center_axis',(0.,-1.,0.));
#8432=DIRECTION('ref_axis',(-0.987688340595138,0.,-0.156434465040231));
#8433=DIRECTION('center_axis',(0.,1.,0.));
#8434=DIRECTION('ref_axis',(1.,0.,0.));
#8435=DIRECTION('center_axis',(0.,-1.,0.));
#8436=DIRECTION('ref_axis',(-1.,0.,-1.22464679914735E-16));
#8437=DIRECTION('center_axis',(0.,1.,0.));
#8438=DIRECTION('ref_axis',(1.,0.,0.));
#8439=DIRECTION('center_axis',(0.,-1.,0.));
#8440=DIRECTION('ref_axis',(-0.987688340595138,0.,0.156434465040231));
#8441=DIRECTION('center_axis',(0.,1.,0.));
#8442=DIRECTION('ref_axis',(1.,0.,0.));
#8443=DIRECTION('center_axis',(0.,-1.,0.));
#8444=DIRECTION('ref_axis',(-0.951056516295154,0.,0.309016994374947));
#8445=DIRECTION('center_axis',(0.,1.,0.));
#8446=DIRECTION('ref_axis',(1.,0.,0.));
#8447=DIRECTION('center_axis',(0.,-1.,0.));
#8448=DIRECTION('ref_axis',(-0.891006524188368,0.,0.453990499739547));
#8449=DIRECTION('center_axis',(0.,1.,0.));
#8450=DIRECTION('ref_axis',(1.,0.,0.));
#8451=DIRECTION('center_axis',(0.,-1.,0.));
#8452=DIRECTION('ref_axis',(-0.809016994374947,0.,0.587785252292473));
#8453=DIRECTION('center_axis',(0.,1.,0.));
#8454=DIRECTION('ref_axis',(1.,0.,0.));
#8455=DIRECTION('center_axis',(0.,-1.,0.));
#8456=DIRECTION('ref_axis',(-0.707106781186548,0.,0.707106781186547));
#8457=DIRECTION('center_axis',(0.,1.,0.));
#8458=DIRECTION('ref_axis',(1.,0.,0.));
#8459=DIRECTION('center_axis',(0.,-1.,0.));
#8460=DIRECTION('ref_axis',(-0.587785252292473,0.,0.809016994374947));
#8461=DIRECTION('center_axis',(0.,1.,0.));
#8462=DIRECTION('ref_axis',(1.,0.,0.));
#8463=DIRECTION('center_axis',(0.,-1.,0.));
#8464=DIRECTION('ref_axis',(-0.453990499739547,0.,0.891006524188368));
#8465=DIRECTION('center_axis',(0.,1.,0.));
#8466=DIRECTION('ref_axis',(1.,0.,0.));
#8467=DIRECTION('center_axis',(0.,-1.,0.));
#8468=DIRECTION('ref_axis',(-0.309016994374948,0.,0.951056516295154));
#8469=DIRECTION('center_axis',(0.,1.,0.));
#8470=DIRECTION('ref_axis',(1.,0.,0.));
#8471=DIRECTION('center_axis',(0.,-1.,0.));
#8472=DIRECTION('ref_axis',(-0.156434465040231,0.,0.987688340595138));
#8473=DIRECTION('center_axis',(0.,1.,0.));
#8474=DIRECTION('ref_axis',(1.,0.,0.));
#8475=DIRECTION('center_axis',(0.,-1.,0.));
#8476=DIRECTION('ref_axis',(-1.83697019872103E-16,0.,1.));
#8477=DIRECTION('center_axis',(0.,1.,0.));
#8478=DIRECTION('ref_axis',(1.,0.,0.));
#8479=DIRECTION('center_axis',(0.,-1.,0.));
#8480=DIRECTION('ref_axis',(0.156434465040231,0.,0.987688340595138));
#8481=DIRECTION('center_axis',(0.,1.,0.));
#8482=DIRECTION('ref_axis',(1.,0.,0.));
#8483=DIRECTION('center_axis',(0.,-1.,0.));
#8484=DIRECTION('ref_axis',(0.309016994374947,0.,0.951056516295154));
#8485=DIRECTION('center_axis',(0.,1.,0.));
#8486=DIRECTION('ref_axis',(1.,0.,0.));
#8487=DIRECTION('center_axis',(0.,-1.,0.));
#8488=DIRECTION('ref_axis',(0.453990499739547,0.,0.891006524188368));
#8489=DIRECTION('center_axis',(0.,1.,0.));
#8490=DIRECTION('ref_axis',(1.,0.,0.));
#8491=DIRECTION('center_axis',(0.,-1.,0.));
#8492=DIRECTION('ref_axis',(0.587785252292473,0.,0.809016994374948));
#8493=DIRECTION('center_axis',(0.,1.,0.));
#8494=DIRECTION('ref_axis',(1.,0.,0.));
#8495=DIRECTION('center_axis',(0.,-1.,0.));
#8496=DIRECTION('ref_axis',(0.707106781186547,0.,0.707106781186548));
#8497=DIRECTION('center_axis',(0.,1.,0.));
#8498=DIRECTION('ref_axis',(1.,0.,0.));
#8499=DIRECTION('center_axis',(0.,-1.,0.));
#8500=DIRECTION('ref_axis',(0.809016994374947,0.,0.587785252292473));
#8501=DIRECTION('center_axis',(0.,1.,0.));
#8502=DIRECTION('ref_axis',(1.,0.,0.));
#8503=DIRECTION('center_axis',(0.,-1.,0.));
#8504=DIRECTION('ref_axis',(0.891006524188368,0.,0.453990499739547));
#8505=DIRECTION('center_axis',(0.,1.,0.));
#8506=DIRECTION('ref_axis',(1.,0.,0.));
#8507=DIRECTION('center_axis',(0.,-1.,0.));
#8508=DIRECTION('ref_axis',(0.951056516295154,0.,0.309016994374948));
#8509=DIRECTION('center_axis',(0.,1.,0.));
#8510=DIRECTION('ref_axis',(1.,0.,0.));
#8511=DIRECTION('center_axis',(0.,1.,0.));
#8512=DIRECTION('ref_axis',(1.,0.,0.));
#8513=DIRECTION('',(0.,-1.,0.));
#8514=DIRECTION('center_axis',(0.,1.,0.));
#8515=DIRECTION('ref_axis',(-0.987688340595137,0.,-0.156434465040233));
#8516=DIRECTION('',(0.,-1.,0.));
#8517=DIRECTION('',(0.,1.,0.));
#8518=DIRECTION('center_axis',(0.,1.,0.));
#8519=DIRECTION('ref_axis',(1.,0.,0.));
#8520=DIRECTION('',(0.,-1.,0.));
#8521=DIRECTION('center_axis',(0.,1.,0.));
#8522=DIRECTION('ref_axis',(-0.951056516295153,0.,-0.309016994374949));
#8523=DIRECTION('',(0.,1.,0.));
#8524=DIRECTION('center_axis',(0.,1.,0.));
#8525=DIRECTION('ref_axis',(1.,0.,0.));
#8526=DIRECTION('',(0.,-1.,0.));
#8527=DIRECTION('center_axis',(0.,1.,0.));
#8528=DIRECTION('ref_axis',(-0.891006524188368,0.,-0.453990499739547));
#8529=DIRECTION('',(0.,1.,0.));
#8530=DIRECTION('center_axis',(0.,1.,0.));
#8531=DIRECTION('ref_axis',(1.,0.,0.));
#8532=DIRECTION('',(0.,-1.,0.));
#8533=DIRECTION('center_axis',(0.,1.,0.));
#8534=DIRECTION('ref_axis',(-0.809016994374948,0.,-0.587785252292473));
#8535=DIRECTION('',(0.,1.,0.));
#8536=DIRECTION('center_axis',(0.,1.,0.));
#8537=DIRECTION('ref_axis',(1.,0.,0.));
#8538=DIRECTION('',(0.,-1.,0.));
#8539=DIRECTION('center_axis',(0.,1.,0.));
#8540=DIRECTION('ref_axis',(-0.707106781186547,0.,-0.707106781186548));
#8541=DIRECTION('',(0.,1.,0.));
#8542=DIRECTION('center_axis',(0.,1.,0.));
#8543=DIRECTION('ref_axis',(1.,0.,0.));
#8544=DIRECTION('',(0.,-1.,0.));
#8545=DIRECTION('center_axis',(0.,1.,0.));
#8546=DIRECTION('ref_axis',(-0.587785252292474,0.,-0.809016994374947));
#8547=DIRECTION('',(0.,1.,0.));
#8548=DIRECTION('center_axis',(0.,1.,0.));
#8549=DIRECTION('ref_axis',(1.,0.,0.));
#8550=DIRECTION('',(0.,-1.,0.));
#8551=DIRECTION('center_axis',(0.,1.,0.));
#8552=DIRECTION('ref_axis',(-0.453990499739547,0.,-0.891006524188368));
#8553=DIRECTION('',(0.,1.,0.));
#8554=DIRECTION('center_axis',(0.,1.,0.));
#8555=DIRECTION('ref_axis',(1.,0.,0.));
#8556=DIRECTION('',(0.,-1.,0.));
#8557=DIRECTION('center_axis',(0.,1.,0.));
#8558=DIRECTION('ref_axis',(-0.309016994374948,0.,-0.951056516295153));
#8559=DIRECTION('',(0.,1.,0.));
#8560=DIRECTION('center_axis',(0.,1.,0.));
#8561=DIRECTION('ref_axis',(1.,0.,0.));
#8562=DIRECTION('',(0.,-1.,0.));
#8563=DIRECTION('center_axis',(0.,1.,0.));
#8564=DIRECTION('ref_axis',(-0.156434465040232,0.,-0.987688340595138));
#8565=DIRECTION('',(0.,1.,0.));
#8566=DIRECTION('center_axis',(0.,1.,0.));
#8567=DIRECTION('ref_axis',(1.,0.,0.));
#8568=DIRECTION('',(0.,-1.,0.));
#8569=DIRECTION('center_axis',(0.,1.,0.));
#8570=DIRECTION('ref_axis',(3.06161699786838E-16,0.,-1.));
#8571=DIRECTION('',(0.,1.,0.));
#8572=DIRECTION('center_axis',(0.,1.,0.));
#8573=DIRECTION('ref_axis',(1.,0.,0.));
#8574=DIRECTION('',(0.,-1.,0.));
#8575=DIRECTION('center_axis',(0.,1.,0.));
#8576=DIRECTION('ref_axis',(0.156434465040233,0.,-0.987688340595138));
#8577=DIRECTION('',(0.,1.,0.));
#8578=DIRECTION('center_axis',(0.,1.,0.));
#8579=DIRECTION('ref_axis',(1.,0.,0.));
#8580=DIRECTION('',(0.,-1.,0.));
#8581=DIRECTION('center_axis',(0.,1.,0.));
#8582=DIRECTION('ref_axis',(0.309016994374946,0.,-0.951056516295154));
#8583=DIRECTION('',(0.,1.,0.));
#8584=DIRECTION('center_axis',(0.,1.,0.));
#8585=DIRECTION('ref_axis',(1.,0.,0.));
#8586=DIRECTION('',(0.,-1.,0.));
#8587=DIRECTION('center_axis',(0.,1.,0.));
#8588=DIRECTION('ref_axis',(0.453990499739547,0.,-0.891006524188368));
#8589=DIRECTION('',(0.,1.,0.));
#8590=DIRECTION('center_axis',(0.,1.,0.));
#8591=DIRECTION('ref_axis',(1.,0.,0.));
#8592=DIRECTION('',(0.,-1.,0.));
#8593=DIRECTION('center_axis',(0.,1.,0.));
#8594=DIRECTION('ref_axis',(0.587785252292473,0.,-0.809016994374947));
#8595=DIRECTION('',(0.,1.,0.));
#8596=DIRECTION('center_axis',(0.,1.,0.));
#8597=DIRECTION('ref_axis',(1.,0.,0.));
#8598=DIRECTION('',(0.,-1.,0.));
#8599=DIRECTION('center_axis',(0.,1.,0.));
#8600=DIRECTION('ref_axis',(0.707106781186548,0.,-0.707106781186547));
#8601=DIRECTION('',(0.,1.,0.));
#8602=DIRECTION('center_axis',(0.,1.,0.));
#8603=DIRECTION('ref_axis',(1.,0.,0.));
#8604=DIRECTION('',(0.,-1.,0.));
#8605=DIRECTION('center_axis',(0.,1.,0.));
#8606=DIRECTION('ref_axis',(0.809016994374946,0.,-0.587785252292475));
#8607=DIRECTION('',(0.,1.,0.));
#8608=DIRECTION('center_axis',(0.,1.,0.));
#8609=DIRECTION('ref_axis',(1.,0.,0.));
#8610=DIRECTION('',(0.,-1.,0.));
#8611=DIRECTION('center_axis',(0.,1.,0.));
#8612=DIRECTION('ref_axis',(0.891006524188368,0.,-0.453990499739547));
#8613=DIRECTION('',(0.,1.,0.));
#8614=DIRECTION('center_axis',(0.,1.,0.));
#8615=DIRECTION('ref_axis',(1.,0.,0.));
#8616=DIRECTION('',(0.,-1.,0.));
#8617=DIRECTION('center_axis',(0.,1.,0.));
#8618=DIRECTION('ref_axis',(0.951056516295154,0.,-0.309016994374946));
#8619=DIRECTION('',(0.,1.,0.));
#8620=DIRECTION('center_axis',(0.,1.,0.));
#8621=DIRECTION('ref_axis',(1.,0.,0.));
#8622=DIRECTION('',(0.,-1.,0.));
#8623=DIRECTION('center_axis',(0.,1.,0.));
#8624=DIRECTION('ref_axis',(0.987688340595138,0.,-0.156434465040232));
#8625=DIRECTION('',(0.,1.,0.));
#8626=DIRECTION('center_axis',(0.,1.,0.));
#8627=DIRECTION('ref_axis',(1.,0.,0.));
#8628=DIRECTION('',(0.,-1.,0.));
#8629=DIRECTION('center_axis',(0.,1.,0.));
#8630=DIRECTION('ref_axis',(1.,0.,2.44929359829471E-16));
#8631=DIRECTION('',(0.,1.,0.));
#8632=DIRECTION('center_axis',(0.,1.,0.));
#8633=DIRECTION('ref_axis',(1.,0.,0.));
#8634=DIRECTION('',(0.,-1.,0.));
#8635=DIRECTION('center_axis',(0.,1.,0.));
#8636=DIRECTION('ref_axis',(0.987688340595137,0.,0.156434465040232));
#8637=DIRECTION('',(0.,1.,0.));
#8638=DIRECTION('center_axis',(0.,1.,0.));
#8639=DIRECTION('ref_axis',(1.,0.,0.));
#8640=DIRECTION('',(0.,-1.,0.));
#8641=DIRECTION('center_axis',(0.,1.,0.));
#8642=DIRECTION('ref_axis',(0.951056516295154,0.,0.309016994374946));
#8643=DIRECTION('',(0.,1.,0.));
#8644=DIRECTION('center_axis',(0.,1.,0.));
#8645=DIRECTION('ref_axis',(1.,0.,0.));
#8646=DIRECTION('',(0.,-1.,0.));
#8647=DIRECTION('center_axis',(0.,1.,0.));
#8648=DIRECTION('ref_axis',(0.891006524188368,0.,0.453990499739547));
#8649=DIRECTION('',(0.,1.,0.));
#8650=DIRECTION('center_axis',(0.,1.,0.));
#8651=DIRECTION('ref_axis',(1.,0.,0.));
#8652=DIRECTION('',(0.,-1.,0.));
#8653=DIRECTION('center_axis',(0.,1.,0.));
#8654=DIRECTION('ref_axis',(0.809016994374947,0.,0.587785252292473));
#8655=DIRECTION('',(0.,1.,0.));
#8656=DIRECTION('center_axis',(0.,1.,0.));
#8657=DIRECTION('ref_axis',(1.,0.,0.));
#8658=DIRECTION('',(0.,-1.,0.));
#8659=DIRECTION('center_axis',(0.,1.,0.));
#8660=DIRECTION('ref_axis',(0.707106781186547,0.,0.707106781186548));
#8661=DIRECTION('',(0.,1.,0.));
#8662=DIRECTION('center_axis',(0.,1.,0.));
#8663=DIRECTION('ref_axis',(1.,0.,0.));
#8664=DIRECTION('',(0.,-1.,0.));
#8665=DIRECTION('center_axis',(0.,1.,0.));
#8666=DIRECTION('ref_axis',(0.587785252292475,0.,0.809016994374946));
#8667=DIRECTION('',(0.,1.,0.));
#8668=DIRECTION('center_axis',(0.,1.,0.));
#8669=DIRECTION('ref_axis',(1.,0.,0.));
#8670=DIRECTION('',(0.,-1.,0.));
#8671=DIRECTION('center_axis',(0.,1.,0.));
#8672=DIRECTION('ref_axis',(0.453990499739547,0.,0.891006524188368));
#8673=DIRECTION('',(0.,1.,0.));
#8674=DIRECTION('center_axis',(0.,1.,0.));
#8675=DIRECTION('ref_axis',(1.,0.,0.));
#8676=DIRECTION('',(0.,-1.,0.));
#8677=DIRECTION('center_axis',(0.,1.,0.));
#8678=DIRECTION('ref_axis',(0.309016994374946,0.,0.951056516295154));
#8679=DIRECTION('',(0.,1.,0.));
#8680=DIRECTION('center_axis',(0.,1.,0.));
#8681=DIRECTION('ref_axis',(1.,0.,0.));
#8682=DIRECTION('',(0.,-1.,0.));
#8683=DIRECTION('center_axis',(0.,1.,0.));
#8684=DIRECTION('ref_axis',(0.156434465040232,0.,0.987688340595138));
#8685=DIRECTION('',(0.,1.,0.));
#8686=DIRECTION('center_axis',(0.,1.,0.));
#8687=DIRECTION('ref_axis',(1.,0.,0.));
#8688=DIRECTION('',(0.,-1.,0.));
#8689=DIRECTION('center_axis',(0.,1.,0.));
#8690=DIRECTION('ref_axis',(-1.83697019872103E-16,0.,1.));
#8691=DIRECTION('',(0.,1.,0.));
#8692=DIRECTION('center_axis',(0.,1.,0.));
#8693=DIRECTION('ref_axis',(1.,0.,0.));
#8694=DIRECTION('',(0.,-1.,0.));
#8695=DIRECTION('center_axis',(0.,1.,0.));
#8696=DIRECTION('ref_axis',(-0.156434465040232,0.,0.987688340595138));
#8697=DIRECTION('',(0.,1.,0.));
#8698=DIRECTION('center_axis',(0.,1.,0.));
#8699=DIRECTION('ref_axis',(1.,0.,0.));
#8700=DIRECTION('',(0.,-1.,0.));
#8701=DIRECTION('center_axis',(0.,1.,0.));
#8702=DIRECTION('ref_axis',(-0.309016994374946,0.,0.951056516295154));
#8703=DIRECTION('',(0.,1.,0.));
#8704=DIRECTION('center_axis',(0.,1.,0.));
#8705=DIRECTION('ref_axis',(1.,0.,0.));
#8706=DIRECTION('',(0.,-1.,0.));
#8707=DIRECTION('center_axis',(0.,1.,0.));
#8708=DIRECTION('ref_axis',(-0.453990499739549,0.,0.891006524188367));
#8709=DIRECTION('',(0.,1.,0.));
#8710=DIRECTION('center_axis',(0.,1.,0.));
#8711=DIRECTION('ref_axis',(1.,0.,0.));
#8712=DIRECTION('',(0.,-1.,0.));
#8713=DIRECTION('center_axis',(0.,1.,0.));
#8714=DIRECTION('ref_axis',(-0.587785252292474,0.,0.809016994374947));
#8715=DIRECTION('',(0.,1.,0.));
#8716=DIRECTION('center_axis',(0.,1.,0.));
#8717=DIRECTION('ref_axis',(1.,0.,0.));
#8718=DIRECTION('',(0.,-1.,0.));
#8719=DIRECTION('center_axis',(0.,1.,0.));
#8720=DIRECTION('ref_axis',(-0.707106781186548,0.,0.707106781186547));
#8721=DIRECTION('',(0.,1.,0.));
#8722=DIRECTION('center_axis',(0.,1.,0.));
#8723=DIRECTION('ref_axis',(1.,0.,0.));
#8724=DIRECTION('',(0.,-1.,0.));
#8725=DIRECTION('center_axis',(0.,1.,0.));
#8726=DIRECTION('ref_axis',(-0.809016994374947,0.,0.587785252292474));
#8727=DIRECTION('',(0.,1.,0.));
#8728=DIRECTION('center_axis',(0.,1.,0.));
#8729=DIRECTION('ref_axis',(1.,0.,0.));
#8730=DIRECTION('',(0.,-1.,0.));
#8731=DIRECTION('center_axis',(0.,1.,0.));
#8732=DIRECTION('ref_axis',(-0.891006524188368,0.,0.453990499739547));
#8733=DIRECTION('',(0.,1.,0.));
#8734=DIRECTION('center_axis',(0.,1.,0.));
#8735=DIRECTION('ref_axis',(1.,0.,0.));
#8736=DIRECTION('',(0.,-1.,0.));
#8737=DIRECTION('center_axis',(0.,1.,0.));
#8738=DIRECTION('ref_axis',(-0.951056516295154,0.,0.309016994374948));
#8739=DIRECTION('',(0.,1.,0.));
#8740=DIRECTION('center_axis',(0.,1.,0.));
#8741=DIRECTION('ref_axis',(1.,0.,0.));
#8742=DIRECTION('',(0.,-1.,0.));
#8743=DIRECTION('center_axis',(0.,1.,0.));
#8744=DIRECTION('ref_axis',(-0.987688340595137,0.,0.156434465040233));
#8745=DIRECTION('',(0.,1.,0.));
#8746=DIRECTION('center_axis',(0.,1.,0.));
#8747=DIRECTION('ref_axis',(1.,0.,0.));
#8748=DIRECTION('',(0.,1.,0.));
#8749=DIRECTION('center_axis',(0.,1.,0.));
#8750=DIRECTION('ref_axis',(-1.,0.,-1.22464679914735E-16));
#8751=DIRECTION('',(0.,-1.,0.));
#8752=DIRECTION('center_axis',(0.,1.,0.));
#8753=DIRECTION('ref_axis',(1.,0.,0.));
#8754=DIRECTION('axis',(0.,0.,1.));
#8755=DIRECTION('refdir',(1.,0.,0.));
#8756=DIRECTION('center_axis',(1.,0.,0.));
#8757=DIRECTION('ref_axis',(0.,0.,-1.));
#8758=DIRECTION('',(0.,0.707106781186547,-0.707106781186548));
#8759=DIRECTION('',(0.,1.,0.));
#8760=DIRECTION('',(0.,0.707106781186547,0.707106781186548));
#8761=DIRECTION('',(0.,0.,1.));
#8762=DIRECTION('',(0.,-0.707106781186548,0.707106781186548));
#8763=DIRECTION('',(0.,-1.,0.));
#8764=DIRECTION('',(0.,-0.707106781186548,-0.707106781186548));
#8765=DIRECTION('',(0.,0.,-1.));
#8766=DIRECTION('center_axis',(0.,-0.707106781186548,-0.707106781186548));
#8767=DIRECTION('ref_axis',(-1.,0.,0.));
#8768=DIRECTION('',(-1.,0.,0.));
#8769=DIRECTION('',(0.,0.707106781186548,-0.707106781186548));
#8770=DIRECTION('',(1.,0.,0.));
#8771=DIRECTION('center_axis',(0.,-1.,0.));
#8772=DIRECTION('ref_axis',(1.,0.,0.));
#8773=DIRECTION('',(1.,0.,0.));
#8774=DIRECTION('',(0.,0.,-1.));
#8775=DIRECTION('center_axis',(0.,-0.707106781186548,0.707106781186547));
#8776=DIRECTION('ref_axis',(1.,0.,0.));
#8777=DIRECTION('',(-1.,0.,0.));
#8778=DIRECTION('',(0.,-0.707106781186547,-0.707106781186548));
#8779=DIRECTION('center_axis',(0.,0.,1.));
#8780=DIRECTION('ref_axis',(1.,0.,0.));
#8781=DIRECTION('',(1.,0.,0.));
#8782=DIRECTION('',(0.,-1.,0.));
#8783=DIRECTION('center_axis',(1.,0.,0.));
#8784=DIRECTION('ref_axis',(0.,0.,-1.));
#8785=DIRECTION('',(0.,-0.707106781186547,0.707106781186548));
#8786=DIRECTION('',(0.,0.,1.));
#8787=DIRECTION('',(0.,0.707106781186548,0.707106781186548));
#8788=DIRECTION('',(0.,1.,0.));
#8789=DIRECTION('center_axis',(0.,0.707106781186548,0.707106781186547));
#8790=DIRECTION('ref_axis',(1.,0.,0.));
#8791=DIRECTION('',(-1.,0.,0.));
#8792=DIRECTION('center_axis',(0.,1.,0.));
#8793=DIRECTION('ref_axis',(-1.,0.,0.));
#8794=DIRECTION('',(1.,0.,0.));
#8795=DIRECTION('center_axis',(0.,0.707106781186548,-0.707106781186548));
#8796=DIRECTION('ref_axis',(-1.,0.,0.));
#8797=DIRECTION('',(-1.,0.,0.));
#8798=DIRECTION('center_axis',(0.,0.,1.));
#8799=DIRECTION('ref_axis',(1.,0.,0.));
#8800=DIRECTION('axis',(0.,0.,1.));
#8801=DIRECTION('refdir',(1.,0.,0.));
#8802=DIRECTION('center_axis',(0.,1.,0.));
#8803=DIRECTION('ref_axis',(0.,0.,1.));
#8804=DIRECTION('center_axis',(0.,-1.,0.));
#8805=DIRECTION('ref_axis',(1.,0.,0.));
#8806=DIRECTION('center_axis',(0.,-1.,0.));
#8807=DIRECTION('ref_axis',(1.,0.,0.));
#8808=DIRECTION('center_axis',(0.,-1.,0.));
#8809=DIRECTION('ref_axis',(1.,0.,0.));
#8810=DIRECTION('',(0.707106781186548,0.707106781186547,8.65956056235493E-17));
#8811=DIRECTION('center_axis',(0.,-1.,0.));
#8812=DIRECTION('ref_axis',(1.,0.,0.));
#8813=DIRECTION('center_axis',(0.,-1.,0.));
#8814=DIRECTION('ref_axis',(1.,0.,0.));
#8815=DIRECTION('',(0.,1.,0.));
#8816=DIRECTION('center_axis',(0.,1.,0.));
#8817=DIRECTION('ref_axis',(1.,0.,0.));
#8818=DIRECTION('center_axis',(0.,-1.,0.));
#8819=DIRECTION('ref_axis',(1.,0.,0.));
#8820=DIRECTION('',(-0.707106781186547,0.707106781186548,-8.65956056235493E-17));
#8821=DIRECTION('center_axis',(0.,-1.,0.));
#8822=DIRECTION('ref_axis',(0.,0.,-1.));
#8823=DIRECTION('center_axis',(0.,-1.,0.));
#8824=DIRECTION('ref_axis',(1.,0.,0.));
#8825=DIRECTION('center_axis',(0.,1.,0.));
#8826=DIRECTION('ref_axis',(1.,0.,0.));
#8827=DIRECTION('center_axis',(0.,1.,0.));
#8828=DIRECTION('ref_axis',(1.,0.,0.));
#8829=DIRECTION('',(-0.447213595499958,0.894427190999916,-5.47678698264203E-17));
#8830=DIRECTION('center_axis',(0.,-1.,0.));
#8831=DIRECTION('ref_axis',(1.,0.,0.));
#8832=DIRECTION('center_axis',(0.,1.,0.));
#8833=DIRECTION('ref_axis',(1.,0.,0.));
#8834=DIRECTION('',(0.,1.,0.));
#8835=DIRECTION('center_axis',(0.,1.,0.));
#8836=DIRECTION('ref_axis',(1.,0.,0.));
#8837=DIRECTION('center_axis',(0.,-1.,0.));
#8838=DIRECTION('ref_axis',(1.,0.,0.));
#8839=DIRECTION('',(-0.707106781186547,0.707106781186548,-8.65956056235493E-17));
#8840=DIRECTION('center_axis',(0.,-1.,0.));
#8841=DIRECTION('ref_axis',(0.,0.,-1.));
#8842=DIRECTION('center_axis',(0.866025403784439,0.,-0.5));
#8843=DIRECTION('ref_axis',(0.5,0.,0.866025403784439));
#8844=DIRECTION('',(-0.5,0.,-0.866025403784439));
#8845=DIRECTION('',(0.,-1.,0.));
#8846=DIRECTION('',(0.5,0.,0.866025403784439));
#8847=DIRECTION('',(0.,-1.,0.));
#8848=DIRECTION('center_axis',(1.20185167898973E-16,0.,-1.));
#8849=DIRECTION('ref_axis',(1.,0.,1.20185167898973E-16));
#8850=DIRECTION('',(-1.,0.,-1.20185167898973E-16));
#8851=DIRECTION('',(0.,-1.,0.));
#8852=DIRECTION('',(1.,0.,1.20185167898973E-16));
#8853=DIRECTION('center_axis',(-0.866025403784439,0.,-0.5));
#8854=DIRECTION('ref_axis',(0.5,0.,-0.866025403784439));
#8855=DIRECTION('',(-0.5,0.,0.866025403784439));
#8856=DIRECTION('',(0.,-1.,0.));
#8857=DIRECTION('',(0.5,0.,-0.866025403784439));
#8858=DIRECTION('center_axis',(-0.866025403784439,0.,0.5));
#8859=DIRECTION('ref_axis',(-0.5,0.,-0.866025403784439));
#8860=DIRECTION('',(0.5,0.,0.866025403784439));
#8861=DIRECTION('',(0.,-1.,0.));
#8862=DIRECTION('',(-0.5,0.,-0.866025403784439));
#8863=DIRECTION('center_axis',(-2.40370335797945E-16,0.,1.));
#8864=DIRECTION('ref_axis',(-1.,0.,-2.40370335797945E-16));
#8865=DIRECTION('',(1.,0.,2.40370335797945E-16));
#8866=DIRECTION('',(0.,-1.,0.));
#8867=DIRECTION('',(-1.,0.,-2.40370335797945E-16));
#8868=DIRECTION('center_axis',(0.866025403784439,0.,0.5));
#8869=DIRECTION('ref_axis',(-0.5,0.,0.866025403784439));
#8870=DIRECTION('',(0.5,0.,-0.866025403784439));
#8871=DIRECTION('',(-0.5,0.,0.866025403784439));
#8872=DIRECTION('center_axis',(0.,1.,0.));
#8873=DIRECTION('ref_axis',(1.,0.,0.));
#8874=DIRECTION('center_axis',(0.,-1.,0.));
#8875=DIRECTION('ref_axis',(0.,0.,-1.));
#8876=DIRECTION('axis',(0.,0.,1.));
#8877=DIRECTION('refdir',(1.,0.,0.));
#8878=DIRECTION('center_axis',(0.866025403784439,0.,-0.5));
#8879=DIRECTION('ref_axis',(0.5,0.,0.866025403784439));
#8880=DIRECTION('',(0.5,0.,0.866025403784439));
#8881=DIRECTION('',(0.,-1.,0.));
#8882=DIRECTION('',(0.5,0.,0.866025403784439));
#8883=DIRECTION('',(0.,-1.,0.));
#8884=DIRECTION('center_axis',(1.92296268638356E-16,0.,-1.));
#8885=DIRECTION('ref_axis',(1.,0.,1.92296268638356E-16));
#8886=DIRECTION('',(1.,0.,1.92296268638356E-16));
#8887=DIRECTION('',(0.,-1.,0.));
#8888=DIRECTION('',(1.,0.,1.92296268638356E-16));
#8889=DIRECTION('center_axis',(-0.866025403784439,0.,-0.5));
#8890=DIRECTION('ref_axis',(0.5,0.,-0.866025403784439));
#8891=DIRECTION('',(0.5,0.,-0.866025403784439));
#8892=DIRECTION('',(0.,-1.,0.));
#8893=DIRECTION('',(0.5,0.,-0.866025403784438));
#8894=DIRECTION('center_axis',(-0.866025403784439,0.,0.5));
#8895=DIRECTION('ref_axis',(-0.5,0.,-0.866025403784439));
#8896=DIRECTION('',(-0.5,0.,-0.866025403784439));
#8897=DIRECTION('',(0.,-1.,0.));
#8898=DIRECTION('',(-0.5,0.,-0.866025403784439));
#8899=DIRECTION('center_axis',(-1.92296268638356E-16,0.,1.));
#8900=DIRECTION('ref_axis',(-1.,0.,-1.92296268638356E-16));
#8901=DIRECTION('',(-1.,0.,-1.92296268638356E-16));
#8902=DIRECTION('',(0.,-1.,0.));
#8903=DIRECTION('',(-1.,0.,-1.92296268638356E-16));
#8904=DIRECTION('center_axis',(0.866025403784439,0.,0.5));
#8905=DIRECTION('ref_axis',(-0.5,0.,0.866025403784439));
#8906=DIRECTION('',(-0.5,0.,0.866025403784439));
#8907=DIRECTION('',(-0.5,0.,0.866025403784439));
#8908=DIRECTION('center_axis',(0.,-1.,0.));
#8909=DIRECTION('ref_axis',(0.,0.,-1.));
#8910=DIRECTION('center_axis',(0.,1.,0.));
#8911=DIRECTION('ref_axis',(0.,0.,1.));
#8912=DIRECTION('center_axis',(0.,-1.,0.));
#8913=DIRECTION('ref_axis',(1.,0.,0.));
#8914=DIRECTION('center_axis',(0.,-1.,0.));
#8915=DIRECTION('ref_axis',(1.,0.,0.));
#8916=DIRECTION('center_axis',(0.,-1.,0.));
#8917=DIRECTION('ref_axis',(1.,0.,0.));
#8918=DIRECTION('',(0.707106781186547,0.707106781186548,8.65956056235493E-17));
#8919=DIRECTION('center_axis',(0.,-1.,0.));
#8920=DIRECTION('ref_axis',(1.,0.,0.));
#8921=DIRECTION('center_axis',(0.,1.,0.));
#8922=DIRECTION('ref_axis',(1.,0.,0.));
#8923=DIRECTION('',(0.,1.,0.));
#8924=DIRECTION('center_axis',(0.,1.,0.));
#8925=DIRECTION('ref_axis',(1.,0.,0.));
#8926=DIRECTION('center_axis',(0.,-1.,0.));
#8927=DIRECTION('ref_axis',(1.,0.,0.));
#8928=DIRECTION('',(-0.707106781186547,0.707106781186548,-8.65956056235493E-17));
#8929=DIRECTION('center_axis',(0.,-1.,0.));
#8930=DIRECTION('ref_axis',(0.,0.,-1.));
#8931=DIRECTION('axis',(0.,0.,1.));
#8932=DIRECTION('refdir',(1.,0.,0.));
#8933=DIRECTION('center_axis',(1.,0.,0.));
#8934=DIRECTION('ref_axis',(0.,0.,-1.));
#8935=DIRECTION('',(0.,-0.707106781186547,-0.707106781186548));
#8936=DIRECTION('',(0.,-1.,0.));
#8937=DIRECTION('',(0.,-0.707106781186547,0.707106781186548));
#8938=DIRECTION('',(0.,0.,1.));
#8939=DIRECTION('',(0.,0.707106781186547,0.707106781186548));
#8940=DIRECTION('',(0.,1.,0.));
#8941=DIRECTION('',(0.,0.707106781186547,-0.707106781186548));
#8942=DIRECTION('',(0.,0.,-1.));
#8943=DIRECTION('center_axis',(0.,0.707106781186548,-0.707106781186547));
#8944=DIRECTION('ref_axis',(-1.,0.,0.));
#8945=DIRECTION('',(1.,0.,0.));
#8946=DIRECTION('',(0.,-0.707106781186547,-0.707106781186548));
#8947=DIRECTION('',(-1.,0.,0.));
#8948=DIRECTION('center_axis',(0.,1.,0.));
#8949=DIRECTION('ref_axis',(-1.,0.,0.));
#8950=DIRECTION('',(-1.,0.,0.));
#8951=DIRECTION('',(0.,0.,-1.));
#8952=DIRECTION('center_axis',(0.,0.707106781186548,0.707106781186547));
#8953=DIRECTION('ref_axis',(1.,0.,0.));
#8954=DIRECTION('',(1.,0.,0.));
#8955=DIRECTION('',(0.,0.707106781186547,-0.707106781186548));
#8956=DIRECTION('center_axis',(0.,0.,1.));
#8957=DIRECTION('ref_axis',(1.,0.,0.));
#8958=DIRECTION('',(-1.,0.,0.));
#8959=DIRECTION('',(0.,1.,0.));
#8960=DIRECTION('center_axis',(1.,0.,0.));
#8961=DIRECTION('ref_axis',(0.,0.,-1.));
#8962=DIRECTION('',(0.,-0.707106781186547,0.707106781186548));
#8963=DIRECTION('',(0.,-1.,0.));
#8964=DIRECTION('',(0.,0.707106781186547,0.707106781186548));
#8965=DIRECTION('',(0.,0.,1.));
#8966=DIRECTION('center_axis',(0.,0.,1.));
#8967=DIRECTION('ref_axis',(1.,0.,0.));
#8968=DIRECTION('',(1.,0.,0.));
#8969=DIRECTION('center_axis',(0.,-0.707106781186548,0.707106781186547));
#8970=DIRECTION('ref_axis',(1.,0.,0.));
#8971=DIRECTION('',(1.,0.,0.));
#8972=DIRECTION('center_axis',(0.,-0.707106781186548,-0.707106781186547));
#8973=DIRECTION('ref_axis',(-1.,0.,0.));
#8974=DIRECTION('',(-1.,0.,0.));
#8975=DIRECTION('center_axis',(0.,-1.,0.));
#8976=DIRECTION('ref_axis',(1.,0.,0.));
#8977=DIRECTION('axis',(0.,0.,1.));
#8978=DIRECTION('refdir',(1.,0.,0.));
#8979=DIRECTION('center_axis',(0.,1.,0.));
#8980=DIRECTION('ref_axis',(1.,0.,0.));
#8981=DIRECTION('center_axis',(0.,-1.,0.));
#8982=DIRECTION('ref_axis',(1.,0.,0.));
#8983=DIRECTION('',(0.,-1.,0.));
#8984=DIRECTION('center_axis',(0.,-1.,0.));
#8985=DIRECTION('ref_axis',(1.,0.,0.));
#8986=DIRECTION('center_axis',(0.,1.,0.));
#8987=DIRECTION('ref_axis',(1.,0.,0.));
#8988=DIRECTION('center_axis',(0.,1.,0.));
#8989=DIRECTION('ref_axis',(1.,0.,0.));
#8990=DIRECTION('',(0.,-1.,0.));
#8991=DIRECTION('center_axis',(0.,1.,0.));
#8992=DIRECTION('ref_axis',(1.,0.,0.));
#8993=DIRECTION('center_axis',(0.,1.,0.));
#8994=DIRECTION('ref_axis',(1.,0.,0.));
#8995=DIRECTION('center_axis',(0.,1.,0.));
#8996=DIRECTION('ref_axis',(1.,0.,0.));
#8997=DIRECTION('axis',(0.,0.,1.));
#8998=DIRECTION('refdir',(1.,0.,0.));
#8999=DIRECTION('center_axis',(0.,1.,0.));
#9000=DIRECTION('ref_axis',(1.,0.,0.));
#9001=DIRECTION('',(0.866025403784439,-0.5,1.06057523872491E-16));
#9002=DIRECTION('center_axis',(0.,-1.,0.));
#9003=DIRECTION('ref_axis',(1.,0.,0.));
#9004=DIRECTION('center_axis',(0.,-1.,0.));
#9005=DIRECTION('ref_axis',(1.,0.,0.));
#9006=DIRECTION('center_axis',(0.,1.,0.));
#9007=DIRECTION('ref_axis',(1.,0.,0.));
#9008=DIRECTION('',(-0.866025403784439,-0.5,-1.06057523872491E-16));
#9009=DIRECTION('center_axis',(1.4792020664489E-16,0.,-1.));
#9010=DIRECTION('ref_axis',(-1.,0.,-1.4792020664489E-16));
#9011=DIRECTION('',(0.,1.,0.));
#9012=DIRECTION('',(0.,1.,0.));
#9013=DIRECTION('center_axis',(-0.866025403784439,0.,-0.5));
#9014=DIRECTION('ref_axis',(-0.5,0.,0.866025403784439));
#9015=DIRECTION('',(0.,1.,0.));
#9016=DIRECTION('center_axis',(-0.866025403784439,0.,0.5));
#9017=DIRECTION('ref_axis',(0.5,0.,0.866025403784439));
#9018=DIRECTION('',(0.,1.,0.));
#9019=DIRECTION('center_axis',(0.,1.,0.));
#9020=DIRECTION('ref_axis',(1.,0.,0.));
#9021=DIRECTION('center_axis',(0.,1.,0.));
#9022=DIRECTION('ref_axis',(1.,0.,0.));
#9023=DIRECTION('',(0.,-1.,0.));
#9024=DIRECTION('center_axis',(0.,1.,0.));
#9025=DIRECTION('ref_axis',(1.,0.,0.));
#9026=DIRECTION('center_axis',(-2.95840413289779E-16,0.,1.));
#9027=DIRECTION('ref_axis',(1.,0.,2.95840413289779E-16));
#9028=DIRECTION('',(0.,1.,0.));
#9029=DIRECTION('center_axis',(0.866025403784439,0.,-0.5));
#9030=DIRECTION('ref_axis',(-0.5,0.,-0.866025403784439));
#9031=DIRECTION('',(0.,1.,0.));
#9032=DIRECTION('center_axis',(0.866025403784439,0.,0.5));
#9033=DIRECTION('ref_axis',(0.5,0.,-0.866025403784439));
#9034=DIRECTION('center_axis',(0.,1.,0.));
#9035=DIRECTION('ref_axis',(1.,0.,0.));
#9036=DIRECTION('center_axis',(0.,1.,0.));
#9037=DIRECTION('ref_axis',(1.,0.,0.));
#9038=DIRECTION('',(0.,0.,1.));
#9039=DIRECTION('',(1.,0.,0.));
#9040=DIRECTION('',(0.,0.,1.));
#9041=DIRECTION('',(1.,0.,0.));
#9042=DIRECTION('',(0.,0.,1.));
#9043=DIRECTION('',(1.,0.,0.));
#9044=DIRECTION('',(0.,0.,1.));
#9045=DIRECTION('',(1.,0.,0.));
#9046=DIRECTION('',(0.,0.,1.));
#9047=DIRECTION('',(1.,0.,0.));
#9048=DIRECTION('',(0.,0.,1.));
#9049=DIRECTION('',(1.,0.,0.));
#9050=DIRECTION('',(0.,0.,1.));
#9051=DIRECTION('',(1.,0.,0.));
#9052=DIRECTION('',(0.,0.,1.));
#9053=DIRECTION('',(1.,0.,0.));
#9054=DIRECTION('',(0.,-1.,2.22044604925031E-16));
#9055=DIRECTION('',(1.,0.,0.));
#9056=DIRECTION('',(0.,-1.,2.22044604925031E-16));
#9057=DIRECTION('',(1.,0.,0.));
#9058=DIRECTION('',(0.,0.,1.));
#9059=DIRECTION('',(1.,0.,0.));
#9060=DIRECTION('',(0.,0.,1.));
#9061=DIRECTION('',(1.,0.,0.));
#9062=DIRECTION('',(0.,0.,1.));
#9063=DIRECTION('',(1.,0.,0.));
#9064=DIRECTION('',(0.,0.,1.));
#9065=DIRECTION('',(1.,0.,0.));
#9066=DIRECTION('',(0.,0.,1.));
#9067=DIRECTION('',(1.,0.,0.));
#9068=DIRECTION('',(0.,0.,1.));
#9069=DIRECTION('',(1.,0.,0.));
#9070=DIRECTION('',(0.,0.,1.));
#9071=DIRECTION('',(1.,0.,0.));
#9072=DIRECTION('',(0.,0.,1.));
#9073=DIRECTION('',(1.,0.,0.));
#9074=DIRECTION('',(0.,0.,1.));
#9075=DIRECTION('',(1.,0.,0.));
#9076=DIRECTION('',(0.,0.,1.));
#9077=DIRECTION('',(1.,0.,0.));
#9078=DIRECTION('',(0.,0.,1.));
#9079=DIRECTION('',(1.,0.,0.));
#9080=DIRECTION('',(0.,0.,1.));
#9081=DIRECTION('',(1.,0.,0.));
#9082=DIRECTION('',(0.,0.,1.));
#9083=DIRECTION('',(1.,0.,0.));
#9084=DIRECTION('',(0.,0.,1.));
#9085=DIRECTION('',(1.,0.,0.));
#9086=DIRECTION('',(0.,0.,1.));
#9087=DIRECTION('',(1.,0.,0.));
#9088=DIRECTION('',(0.,0.,1.));
#9089=DIRECTION('',(1.,0.,0.));
#9090=DIRECTION('',(0.,0.,1.));
#9091=DIRECTION('',(1.,0.,0.));
#9092=DIRECTION('',(0.,0.,1.));
#9093=DIRECTION('',(1.,0.,0.));
#9094=DIRECTION('',(0.,0.,1.));
#9095=DIRECTION('',(1.,0.,0.));
#9096=DIRECTION('',(0.,0.,1.));
#9097=DIRECTION('',(1.,0.,0.));
#9098=DIRECTION('',(0.,0.,1.));
#9099=DIRECTION('',(1.,0.,0.));
#9100=DIRECTION('',(0.,0.,1.));
#9101=DIRECTION('',(1.,0.,0.));
#9102=DIRECTION('',(0.,0.,1.));
#9103=DIRECTION('',(1.,0.,0.));
#9104=DIRECTION('',(0.,0.,1.));
#9105=DIRECTION('',(1.,0.,0.));
#9106=DIRECTION('',(0.,0.,1.));
#9107=DIRECTION('',(1.,0.,0.));
#9108=DIRECTION('',(0.,0.,1.));
#9109=DIRECTION('',(1.,0.,0.));
#9110=DIRECTION('',(8.65956056235493E-17,-8.65956056235493E-17,-1.));
#9111=DIRECTION('',(2.22044604925031E-16,1.,-8.65956056235494E-17));
#9112=DIRECTION('',(0.,0.,1.));
#9113=DIRECTION('',(-1.,1.22464679914735E-16,0.));
#9114=DIRECTION('',(0.,-1.,2.22044604925031E-16));
#9115=DIRECTION('',(1.,0.,0.));
#9116=DIRECTION('',(0.,-1.,2.22044604925031E-16));
#9117=DIRECTION('',(1.,0.,0.));
#9118=DIRECTION('',(8.65956056235493E-17,-8.65956056235493E-17,-1.));
#9119=DIRECTION('',(2.22044604925031E-16,1.,-8.65956056235494E-17));
#9120=DIRECTION('',(0.,0.,1.));
#9121=DIRECTION('',(1.,0.,0.));
#9122=DIRECTION('',(0.,0.,1.));
#9123=DIRECTION('',(1.,0.,0.));
#9124=DIRECTION('',(0.,0.,1.));
#9125=DIRECTION('',(1.,0.,0.));
#9126=DIRECTION('',(0.,0.,1.));
#9127=DIRECTION('',(1.,0.,0.));
#9128=CARTESIAN_POINT('',(0.,0.,0.));
#9129=CARTESIAN_POINT('',(0.,0.,0.));
#9130=CARTESIAN_POINT('',(0.,0.,0.));
#9131=CARTESIAN_POINT('Origin',(-5.,-2.5,-0.1));
#9132=CARTESIAN_POINT('',(-5.25,-2.5,0.));
#9133=CARTESIAN_POINT('Origin',(-5.,-2.5,0.));
#9134=CARTESIAN_POINT('',(-5.25,-2.5,1.2));
#9135=CARTESIAN_POINT('',(-5.25,-2.5,-0.1));
#9136=CARTESIAN_POINT('Origin',(-5.,-2.5,1.2));
#9137=CARTESIAN_POINT('Origin',(5.,-2.5,-0.1));
#9138=CARTESIAN_POINT('',(4.75,-2.5,0.));
#9139=CARTESIAN_POINT('Origin',(5.,-2.5,0.));
#9140=CARTESIAN_POINT('',(4.75,-2.5,1.2));
#9141=CARTESIAN_POINT('',(4.75,-2.5,-0.1));
#9142=CARTESIAN_POINT('Origin',(5.,-2.5,1.2));
#9143=CARTESIAN_POINT('Origin',(8.,4.,0.));
#9144=CARTESIAN_POINT('',(8.,4.,0.));
#9145=CARTESIAN_POINT('',(-8.,4.,0.));
#9146=CARTESIAN_POINT('',(8.,4.,0.));
#9147=CARTESIAN_POINT('',(-8.,4.,1.2));
#9148=CARTESIAN_POINT('',(-8.,4.,0.));
#9149=CARTESIAN_POINT('',(8.,4.,1.2));
#9150=CARTESIAN_POINT('',(8.,4.,1.2));
#9151=CARTESIAN_POINT('',(8.,4.,0.));
#9152=CARTESIAN_POINT('Origin',(8.,-4.,0.));
#9153=CARTESIAN_POINT('',(8.,-4.,0.));
#9154=CARTESIAN_POINT('',(8.,-4.,0.));
#9155=CARTESIAN_POINT('',(8.,-4.,1.2));
#9156=CARTESIAN_POINT('',(8.,-4.,1.2));
#9157=CARTESIAN_POINT('',(8.,-4.,0.));
#9158=CARTESIAN_POINT('Origin',(-8.,-4.,0.));
#9159=CARTESIAN_POINT('',(-8.,-4.,0.));
#9160=CARTESIAN_POINT('',(-8.,-4.,0.));
#9161=CARTESIAN_POINT('',(-8.,-4.,1.2));
#9162=CARTESIAN_POINT('',(-8.,-4.,1.2));
#9163=CARTESIAN_POINT('',(-8.,-4.,0.));
#9164=CARTESIAN_POINT('Origin',(-8.,4.,0.));
#9165=CARTESIAN_POINT('',(-8.,4.,0.));
#9166=CARTESIAN_POINT('',(-8.,4.,1.2));
#9167=CARTESIAN_POINT('Origin',(0.,0.,1.2));
#9168=CARTESIAN_POINT('Origin',(0.,0.,0.));
#9169=CARTESIAN_POINT('',(0.,0.,0.));
#9170=CARTESIAN_POINT('Origin',(-5.,-2.5,1.1));
#9171=CARTESIAN_POINT('',(-5.33,-2.5,1.2));
#9172=CARTESIAN_POINT('Origin',(-5.,-2.5,1.2));
#9173=CARTESIAN_POINT('',(-5.33,-2.5,2.2));
#9174=CARTESIAN_POINT('',(-5.33,-2.5,1.1));
#9175=CARTESIAN_POINT('Origin',(-5.,-2.5,2.2));
#9176=CARTESIAN_POINT('Origin',(5.,-2.5,1.1));
#9177=CARTESIAN_POINT('',(4.67,-2.5,1.2));
#9178=CARTESIAN_POINT('Origin',(5.,-2.5,1.2));
#9179=CARTESIAN_POINT('',(4.67,-2.5,2.2));
#9180=CARTESIAN_POINT('',(4.67,-2.5,1.1));
#9181=CARTESIAN_POINT('Origin',(5.,-2.5,2.2));
#9182=CARTESIAN_POINT('Origin',(3.2,-1.4,4.8));
#9183=CARTESIAN_POINT('',(2.76,-1.3,4.8));
#9184=CARTESIAN_POINT('Origin',(3.2,-1.3,4.8));
#9185=CARTESIAN_POINT('',(2.76,-0.5,4.8));
#9186=CARTESIAN_POINT('',(2.76,-1.4,4.8));
#9187=CARTESIAN_POINT('Origin',(3.2,-0.5,4.8));
#9188=CARTESIAN_POINT('Origin',(-3.2,-1.4,11.2));
#9189=CARTESIAN_POINT('',(-3.64,-1.3,11.2));
#9190=CARTESIAN_POINT('Origin',(-3.2,-1.3,11.2));
#9191=CARTESIAN_POINT('',(-3.64,-0.5,11.2));
#9192=CARTESIAN_POINT('',(-3.64,-1.4,11.2));
#9193=CARTESIAN_POINT('Origin',(-3.2,-0.5,11.2));
#9194=CARTESIAN_POINT('Origin',(-3.2,-1.4,4.8));
#9195=CARTESIAN_POINT('',(-3.64,-1.3,4.8));
#9196=CARTESIAN_POINT('Origin',(-3.2,-1.3,4.8));
#9197=CARTESIAN_POINT('',(-3.64,-0.5,4.8));
#9198=CARTESIAN_POINT('',(-3.64,-1.4,4.8));
#9199=CARTESIAN_POINT('Origin',(-3.2,-0.5,4.8));
#9200=CARTESIAN_POINT('Origin',(3.2,-1.4,11.2));
#9201=CARTESIAN_POINT('',(2.76,-1.3,11.2));
#9202=CARTESIAN_POINT('Origin',(3.2,-1.3,11.2));
#9203=CARTESIAN_POINT('',(2.76,-0.5,11.2));
#9204=CARTESIAN_POINT('',(2.76,-1.4,11.2));
#9205=CARTESIAN_POINT('Origin',(3.2,-0.5,11.2));
#9206=CARTESIAN_POINT('Origin',(0.,-1.4,8.));
#9207=CARTESIAN_POINT('',(-3.1,-1.3,8.));
#9208=CARTESIAN_POINT('Origin',(0.,-1.3,8.));
#9209=CARTESIAN_POINT('',(-3.1,-0.5,8.));
#9210=CARTESIAN_POINT('',(-3.1,-1.4,8.));
#9211=CARTESIAN_POINT('Origin',(0.,-0.5,8.));
#9212=CARTESIAN_POINT('Origin',(-6.5,-3.5,2.2));
#9213=CARTESIAN_POINT('',(-6.5,-1.3,2.2));
#9214=CARTESIAN_POINT('',(6.5,-1.3,2.2));
#9215=CARTESIAN_POINT('',(-6.5,-1.3,2.2));
#9216=CARTESIAN_POINT('',(-6.5,-3.5,2.2));
#9217=CARTESIAN_POINT('',(-6.5,-3.5,2.2));
#9218=CARTESIAN_POINT('',(6.5,-3.5,2.2));
#9219=CARTESIAN_POINT('',(6.5,-3.5,2.2));
#9220=CARTESIAN_POINT('',(6.5,-3.5,2.2));
#9221=CARTESIAN_POINT('Origin',(0.,-3.5,1.7));
#9222=CARTESIAN_POINT('',(-6.5,-3.5,1.2));
#9223=CARTESIAN_POINT('',(-6.5,-3.5,2.2));
#9224=CARTESIAN_POINT('',(6.5,-3.5,1.2));
#9225=CARTESIAN_POINT('',(-6.5,-3.5,1.2));
#9226=CARTESIAN_POINT('',(6.5,-3.5,1.2));
#9227=CARTESIAN_POINT('Origin',(6.5,-0.5,1.2));
#9228=CARTESIAN_POINT('',(-6.5,-0.5,1.2));
#9229=CARTESIAN_POINT('',(-6.5,-0.5,14.5));
#9230=CARTESIAN_POINT('',(-6.5,-0.5,1.2));
#9231=CARTESIAN_POINT('',(6.5,-0.5,14.5));
#9232=CARTESIAN_POINT('',(6.5,-0.5,14.5));
#9233=CARTESIAN_POINT('',(6.5,-0.5,1.2));
#9234=CARTESIAN_POINT('',(6.5,-0.5,1.2));
#9235=CARTESIAN_POINT('',(6.5,-0.5,1.2));
#9236=CARTESIAN_POINT('Origin',(-6.5,-0.5,1.2));
#9237=CARTESIAN_POINT('',(-6.5,-1.3,14.5));
#9238=CARTESIAN_POINT('',(-6.5,-1.3,1.2));
#9239=CARTESIAN_POINT('',(-6.5,-0.5,14.5));
#9240=CARTESIAN_POINT('',(-6.5,-0.5,1.2));
#9241=CARTESIAN_POINT('Origin',(6.5,-1.3,1.2));
#9242=CARTESIAN_POINT('',(6.5,-1.3,14.5));
#9243=CARTESIAN_POINT('',(6.5,-1.3,14.5));
#9244=CARTESIAN_POINT('',(6.5,-1.3,1.2));
#9245=CARTESIAN_POINT('',(6.5,-3.5,1.2));
#9246=CARTESIAN_POINT('Origin',(-6.5,-1.3,1.2));
#9247=CARTESIAN_POINT('',(-6.5,-1.3,14.5));
#9248=CARTESIAN_POINT('Origin',(0.,-0.9,14.5));
#9249=CARTESIAN_POINT('Origin',(0.,-0.9,1.2));
#9250=CARTESIAN_POINT('',(0.,0.,0.));
#9251=CARTESIAN_POINT('Origin',(-3.2,-0.5,4.8));
#9252=CARTESIAN_POINT('',(-3.625,0.5,4.8));
#9253=CARTESIAN_POINT('Origin',(-3.2,0.5,4.8));
#9254=CARTESIAN_POINT('',(-3.625,-0.5,4.8));
#9255=CARTESIAN_POINT('',(-3.625,-0.5,4.8));
#9256=CARTESIAN_POINT('Origin',(-3.2,-0.5,4.8));
#9257=CARTESIAN_POINT('Origin',(-3.2,-0.5,4.8));
#9258=CARTESIAN_POINT('',(-3.795,0.5,4.8));
#9259=CARTESIAN_POINT('Origin',(-3.2,0.5,4.8));
#9260=CARTESIAN_POINT('',(-3.795,-0.5,4.8));
#9261=CARTESIAN_POINT('',(-3.795,-0.5,4.8));
#9262=CARTESIAN_POINT('Origin',(-3.2,-0.5,4.8));
#9263=CARTESIAN_POINT('Origin',(-3.2,0.5,4.8));
#9264=CARTESIAN_POINT('Origin',(-3.2,-0.5,4.8));
#9265=CARTESIAN_POINT('',(0.,0.,0.));
#9266=CARTESIAN_POINT('Origin',(-3.2,-0.5,11.2));
#9267=CARTESIAN_POINT('',(-3.625,0.5,11.2));
#9268=CARTESIAN_POINT('Origin',(-3.2,0.5,11.2));
#9269=CARTESIAN_POINT('',(-3.625,-0.5,11.2));
#9270=CARTESIAN_POINT('',(-3.625,-0.5,11.2));
#9271=CARTESIAN_POINT('Origin',(-3.2,-0.5,11.2));
#9272=CARTESIAN_POINT('Origin',(-3.2,-0.5,11.2));
#9273=CARTESIAN_POINT('',(-3.795,0.5,11.2));
#9274=CARTESIAN_POINT('Origin',(-3.2,0.5,11.2));
#9275=CARTESIAN_POINT('',(-3.795,-0.5,11.2));
#9276=CARTESIAN_POINT('',(-3.795,-0.5,11.2));
#9277=CARTESIAN_POINT('Origin',(-3.2,-0.5,11.2));
#9278=CARTESIAN_POINT('Origin',(-3.2,0.5,11.2));
#9279=CARTESIAN_POINT('Origin',(-3.2,-0.5,11.2));
#9280=CARTESIAN_POINT('',(0.,0.,0.));
#9281=CARTESIAN_POINT('Origin',(3.2,-0.5,4.8));
#9282=CARTESIAN_POINT('',(2.775,0.5,4.8));
#9283=CARTESIAN_POINT('Origin',(3.2,0.5,4.8));
#9284=CARTESIAN_POINT('',(2.775,-0.5,4.8));
#9285=CARTESIAN_POINT('',(2.775,-0.5,4.8));
#9286=CARTESIAN_POINT('Origin',(3.2,-0.5,4.8));
#9287=CARTESIAN_POINT('Origin',(3.2,-0.5,4.8));
#9288=CARTESIAN_POINT('',(2.605,0.5,4.8));
#9289=CARTESIAN_POINT('Origin',(3.2,0.5,4.8));
#9290=CARTESIAN_POINT('',(2.605,-0.5,4.8));
#9291=CARTESIAN_POINT('',(2.605,-0.5,4.8));
#9292=CARTESIAN_POINT('Origin',(3.2,-0.5,4.8));
#9293=CARTESIAN_POINT('Origin',(3.2,0.5,4.8));
#9294=CARTESIAN_POINT('Origin',(3.2,-0.5,4.8));
#9295=CARTESIAN_POINT('',(0.,0.,0.));
#9296=CARTESIAN_POINT('Origin',(3.2,-0.5,11.2));
#9297=CARTESIAN_POINT('',(2.775,0.5,11.2));
#9298=CARTESIAN_POINT('Origin',(3.2,0.5,11.2));
#9299=CARTESIAN_POINT('',(2.775,-0.5,11.2));
#9300=CARTESIAN_POINT('',(2.775,-0.5,11.2));
#9301=CARTESIAN_POINT('Origin',(3.2,-0.5,11.2));
#9302=CARTESIAN_POINT('Origin',(3.2,-0.5,11.2));
#9303=CARTESIAN_POINT('',(2.605,0.5,11.2));
#9304=CARTESIAN_POINT('Origin',(3.2,0.5,11.2));
#9305=CARTESIAN_POINT('',(2.605,-0.5,11.2));
#9306=CARTESIAN_POINT('',(2.605,-0.5,11.2));
#9307=CARTESIAN_POINT('Origin',(3.2,-0.5,11.2));
#9308=CARTESIAN_POINT('Origin',(3.2,0.5,11.2));
#9309=CARTESIAN_POINT('Origin',(3.2,-0.5,11.2));
#9310=CARTESIAN_POINT('',(0.,0.,0.));
#9311=CARTESIAN_POINT('Origin',(8.,-3.,-0.5));
#9312=CARTESIAN_POINT('',(8.,-3.,-0.5));
#9313=CARTESIAN_POINT('',(-8.,-3.,-0.5));
#9314=CARTESIAN_POINT('',(8.,-3.,-0.5));
#9315=CARTESIAN_POINT('',(-8.,-3.,0.));
#9316=CARTESIAN_POINT('',(-8.,-3.,-0.5));
#9317=CARTESIAN_POINT('',(8.,-3.,0.));
#9318=CARTESIAN_POINT('',(8.,-3.,0.));
#9319=CARTESIAN_POINT('',(8.,-3.,-0.5));
#9320=CARTESIAN_POINT('Origin',(8.,-4.,-0.5));
#9321=CARTESIAN_POINT('',(8.,-4.,-0.5));
#9322=CARTESIAN_POINT('',(8.,-4.,-0.5));
#9323=CARTESIAN_POINT('',(8.,-4.,0.));
#9324=CARTESIAN_POINT('',(8.,-4.,0.));
#9325=CARTESIAN_POINT('',(8.,-4.,-0.5));
#9326=CARTESIAN_POINT('Origin',(-8.,-4.,-0.5));
#9327=CARTESIAN_POINT('',(-8.,-4.,-0.5));
#9328=CARTESIAN_POINT('',(-8.,-4.,-0.5));
#9329=CARTESIAN_POINT('',(-8.,-4.,0.));
#9330=CARTESIAN_POINT('',(-8.,-4.,0.));
#9331=CARTESIAN_POINT('',(-8.,-4.,-0.5));
#9332=CARTESIAN_POINT('Origin',(-8.,-3.,-0.5));
#9333=CARTESIAN_POINT('',(-8.,-3.,-0.5));
#9334=CARTESIAN_POINT('',(-8.,-3.,0.));
#9335=CARTESIAN_POINT('Origin',(0.,-3.5,0.));
#9336=CARTESIAN_POINT('Origin',(0.,-3.5,-0.5));
#9337=CARTESIAN_POINT('',(0.,0.,0.));
#9338=CARTESIAN_POINT('Origin',(8.,4.,-0.5));
#9339=CARTESIAN_POINT('',(8.,4.,-0.5));
#9340=CARTESIAN_POINT('',(-8.,4.,-0.5));
#9341=CARTESIAN_POINT('',(8.,4.,-0.5));
#9342=CARTESIAN_POINT('',(-8.,4.,0.));
#9343=CARTESIAN_POINT('',(-8.,4.,-0.5));
#9344=CARTESIAN_POINT('',(8.,4.,0.));
#9345=CARTESIAN_POINT('',(8.,4.,0.));
#9346=CARTESIAN_POINT('',(8.,4.,-0.5));
#9347=CARTESIAN_POINT('Origin',(8.,3.,-0.5));
#9348=CARTESIAN_POINT('',(8.,3.,-0.5));
#9349=CARTESIAN_POINT('',(8.,3.,-0.5));
#9350=CARTESIAN_POINT('',(8.,3.,0.));
#9351=CARTESIAN_POINT('',(8.,3.,0.));
#9352=CARTESIAN_POINT('',(8.,3.,-0.5));
#9353=CARTESIAN_POINT('Origin',(-8.,3.,-0.5));
#9354=CARTESIAN_POINT('',(-8.,3.,-0.5));
#9355=CARTESIAN_POINT('',(-8.,3.,-0.5));
#9356=CARTESIAN_POINT('',(-8.,3.,0.));
#9357=CARTESIAN_POINT('',(-8.,3.,0.));
#9358=CARTESIAN_POINT('',(-8.,3.,-0.5));
#9359=CARTESIAN_POINT('Origin',(-8.,4.,-0.5));
#9360=CARTESIAN_POINT('',(-8.,4.,-0.5));
#9361=CARTESIAN_POINT('',(-8.,4.,0.));
#9362=CARTESIAN_POINT('Origin',(0.,3.5,0.));
#9363=CARTESIAN_POINT('Origin',(0.,3.5,-0.5));
#9364=CARTESIAN_POINT('',(0.,0.,0.));
#9365=CARTESIAN_POINT('Origin',(0.144337567297406,-0.6,-0.25));
#9366=CARTESIAN_POINT('',(0.288675134594813,-0.6,0.));
#9367=CARTESIAN_POINT('',(0.144337567297406,-0.6,-0.25));
#9368=CARTESIAN_POINT('',(0.288675134594813,-0.6,0.));
#9369=CARTESIAN_POINT('',(0.144337567297406,-0.96,-0.25));
#9370=CARTESIAN_POINT('',(0.144337567297406,-0.6,-0.25));
#9371=CARTESIAN_POINT('',(0.288675134594813,-0.96,0.));
#9372=CARTESIAN_POINT('',(0.288675134594813,-0.96,0.));
#9373=CARTESIAN_POINT('',(0.288675134594813,-0.6,0.));
#9374=CARTESIAN_POINT('Origin',(-0.144337567297406,-0.6,-0.25));
#9375=CARTESIAN_POINT('',(-0.144337567297406,-0.6,-0.25));
#9376=CARTESIAN_POINT('',(0.144337567297406,-0.6,-0.25));
#9377=CARTESIAN_POINT('',(-0.144337567297406,-0.96,-0.25));
#9378=CARTESIAN_POINT('',(-0.144337567297406,-0.6,-0.25));
#9379=CARTESIAN_POINT('',(0.144337567297406,-0.96,-0.25));
#9380=CARTESIAN_POINT('Origin',(-0.288675134594813,-0.6,-8.32667268468867E-17));
#9381=CARTESIAN_POINT('',(-0.288675134594813,-0.6,-3.53525079574969E-17));
#9382=CARTESIAN_POINT('',(-0.144337567297406,-0.6,-0.25));
#9383=CARTESIAN_POINT('',(-0.288675134594813,-0.96,-5.55111512312578E-17));
#9384=CARTESIAN_POINT('',(-0.288675134594813,-0.6,-3.53525079574969E-17));
#9385=CARTESIAN_POINT('',(-0.144337567297406,-0.96,-0.25));
#9386=CARTESIAN_POINT('Origin',(-0.144337567297407,-0.6,0.25));
#9387=CARTESIAN_POINT('',(-0.144337567297407,-0.6,0.25));
#9388=CARTESIAN_POINT('',(-0.288675134594813,-0.6,-3.53525079574969E-17));
#9389=CARTESIAN_POINT('',(-0.144337567297407,-0.96,0.25));
#9390=CARTESIAN_POINT('',(-0.144337567297407,-0.6,0.25));
#9391=CARTESIAN_POINT('',(-0.288675134594813,-0.96,-3.53525079574969E-17));
#9392=CARTESIAN_POINT('Origin',(0.144337567297406,-0.6,0.25));
#9393=CARTESIAN_POINT('',(0.144337567297406,-0.6,0.25));
#9394=CARTESIAN_POINT('',(-0.144337567297407,-0.6,0.25));
#9395=CARTESIAN_POINT('',(0.144337567297406,-0.96,0.25));
#9396=CARTESIAN_POINT('',(0.144337567297406,-0.6,0.25));
#9397=CARTESIAN_POINT('',(-0.144337567297407,-0.96,0.25));
#9398=CARTESIAN_POINT('Origin',(0.288675134594813,-0.6,0.));
#9399=CARTESIAN_POINT('',(0.144337567297406,-0.6,0.25));
#9400=CARTESIAN_POINT('',(0.144337567297406,-0.96,0.25));
#9401=CARTESIAN_POINT('Origin',(0.,-0.6,0.));
#9402=CARTESIAN_POINT('Origin',(0.,-0.96,0.));
#9403=CARTESIAN_POINT('Origin',(0.,-1.8,0.));
#9404=CARTESIAN_POINT('',(-0.2942,-1.8,3.60291088309151E-17));
#9405=CARTESIAN_POINT('Origin',(0.,-1.8,0.));
#9406=CARTESIAN_POINT('Origin',(0.45,0.6,0.));
#9407=CARTESIAN_POINT('',(-0.45,0.6,-5.51091059616309E-17));
#9408=CARTESIAN_POINT('Origin',(0.,0.6,0.));
#9409=CARTESIAN_POINT('Origin',(0.,0.575,0.));
#9410=CARTESIAN_POINT('',(-0.5,0.55,-6.12323399573677E-17));
#9411=CARTESIAN_POINT('Origin',(0.,0.55,0.));
#9412=CARTESIAN_POINT('',(-0.475,0.575,-5.81707229594993E-17));
#9413=CARTESIAN_POINT('Origin',(0.,0.29,0.));
#9414=CARTESIAN_POINT('',(-0.5,0.0299999999999998,-6.12323399573677E-17));
#9415=CARTESIAN_POINT('Origin',(0.,0.0299999999999998,0.));
#9416=CARTESIAN_POINT('',(-0.5,0.29,-6.12323399573677E-17));
#9417=CARTESIAN_POINT('Origin',(0.,0.0150000000000001,0.));
#9418=CARTESIAN_POINT('',(-0.47,7.11236625150491E-17,-5.75583995599256E-17));
#9419=CARTESIAN_POINT('Origin',(0.,0.,0.));
#9420=CARTESIAN_POINT('',(-0.485,0.0150000000000001,-5.93953697586466E-17));
#9421=CARTESIAN_POINT('Origin',(0.32,0.,0.));
#9422=CARTESIAN_POINT('',(-0.32,-6.93889390390723E-18,-3.91886975727153E-17));
#9423=CARTESIAN_POINT('Origin',(0.,0.,0.));
#9424=CARTESIAN_POINT('Origin',(0.,-0.02,0.));
#9425=CARTESIAN_POINT('',(-0.2942,-0.0515999999999999,3.60291088309151E-17));
#9426=CARTESIAN_POINT('Origin',(0.,-0.0515999999999999,0.));
#9427=CARTESIAN_POINT('',(-0.31,-0.02,-3.7964050773568E-17));
#9428=CARTESIAN_POINT('Origin',(0.,-1.24,0.));
#9429=CARTESIAN_POINT('',(-0.2942,-1.24,-3.60291088309151E-17));
#9430=CARTESIAN_POINT('',(0.,0.,0.));
#9431=CARTESIAN_POINT('',(0.,0.,0.));
#9432=CARTESIAN_POINT('Origin',(0.,0.,0.));
#9433=CARTESIAN_POINT('',(-2.05,-1.665,2.51052593825207E-16));
#9434=CARTESIAN_POINT('Origin',(0.,-1.665,0.));
#9435=CARTESIAN_POINT('',(-2.05,-1.14891252930761,-2.51052593825207E-16));
#9436=CARTESIAN_POINT('',(-2.05,0.,2.51052593825207E-16));
#9437=CARTESIAN_POINT('Origin',(0.,-1.14891252930761,0.));
#9438=CARTESIAN_POINT('Origin',(0.,0.,0.));
#9439=CARTESIAN_POINT('',(-2.05,1.14891252930761,2.51052593825207E-16));
#9440=CARTESIAN_POINT('Origin',(0.,1.14891252930761,0.));
#9441=CARTESIAN_POINT('',(-2.05,1.665,-2.51052593825207E-16));
#9442=CARTESIAN_POINT('',(-2.05,0.,2.51052593825207E-16));
#9443=CARTESIAN_POINT('Origin',(0.,1.665,0.));
#9444=CARTESIAN_POINT('Origin',(0.,0.,0.));
#9445=CARTESIAN_POINT('',(-1.43895998899814E-16,-1.76221774462768E-32,-2.35));
#9446=CARTESIAN_POINT('',(-1.43895998899814E-16,-1.76221774462768E-32,2.35));
#9447=CARTESIAN_POINT('Origin',(0.,0.,0.));
#9448=CARTESIAN_POINT('Origin',(0.,0.,0.));
#9449=CARTESIAN_POINT('',(-3.,-0.5,3.67394039744206E-16));
#9450=CARTESIAN_POINT('Origin',(0.,-0.5,0.));
#9451=CARTESIAN_POINT('',(-3.,-1.665,3.67394039744206E-16));
#9452=CARTESIAN_POINT('',(-3.,0.,3.67394039744206E-16));
#9453=CARTESIAN_POINT('Origin',(0.,-1.665,0.));
#9454=CARTESIAN_POINT('Origin',(0.,0.,0.));
#9455=CARTESIAN_POINT('',(-3.,1.665,3.67394039744206E-16));
#9456=CARTESIAN_POINT('Origin',(0.,1.665,0.));
#9457=CARTESIAN_POINT('',(-3.,0.5,-3.67394039744206E-16));
#9458=CARTESIAN_POINT('',(-3.,0.,3.67394039744206E-16));
#9459=CARTESIAN_POINT('Origin',(0.,0.5,0.));
#9460=CARTESIAN_POINT('Origin',(0.,-1.665,0.));
#9461=CARTESIAN_POINT('Origin',(0.,1.665,0.));
#9462=CARTESIAN_POINT('Origin',(3.2,0.,3.2));
#9463=CARTESIAN_POINT('',(2.6,-0.5,3.2));
#9464=CARTESIAN_POINT('Origin',(3.2,-0.5,3.2));
#9465=CARTESIAN_POINT('',(2.6,0.5,3.2));
#9466=CARTESIAN_POINT('',(2.6,0.,3.2));
#9467=CARTESIAN_POINT('Origin',(3.2,0.5,3.2));
#9468=CARTESIAN_POINT('Origin',(-3.2,0.,-3.2));
#9469=CARTESIAN_POINT('',(-3.8,-0.5,-3.2));
#9470=CARTESIAN_POINT('Origin',(-3.2,-0.5,-3.2));
#9471=CARTESIAN_POINT('',(-3.8,0.5,-3.2));
#9472=CARTESIAN_POINT('',(-3.8,0.,-3.2));
#9473=CARTESIAN_POINT('Origin',(-3.2,0.5,-3.2));
#9474=CARTESIAN_POINT('Origin',(-3.2,0.,3.2));
#9475=CARTESIAN_POINT('',(-3.8,-0.5,3.2));
#9476=CARTESIAN_POINT('Origin',(-3.2,-0.5,3.2));
#9477=CARTESIAN_POINT('',(-3.8,0.5,3.2));
#9478=CARTESIAN_POINT('',(-3.8,0.,3.2));
#9479=CARTESIAN_POINT('Origin',(-3.2,0.5,3.2));
#9480=CARTESIAN_POINT('Origin',(3.2,0.,-3.2));
#9481=CARTESIAN_POINT('',(2.6,-0.5,-3.2));
#9482=CARTESIAN_POINT('Origin',(3.2,-0.5,-3.2));
#9483=CARTESIAN_POINT('',(2.6,0.5,-3.2));
#9484=CARTESIAN_POINT('',(2.6,0.,-3.2));
#9485=CARTESIAN_POINT('Origin',(3.2,0.5,-3.2));
#9486=CARTESIAN_POINT('Origin',(-4.3,-0.5,-3.3));
#9487=CARTESIAN_POINT('',(-4.3,-0.5,-3.3));
#9488=CARTESIAN_POINT('',(-4.3,-0.5,3.3));
#9489=CARTESIAN_POINT('',(-4.3,-0.5,-3.3));
#9490=CARTESIAN_POINT('',(-4.3,0.5,3.3));
#9491=CARTESIAN_POINT('',(-4.3,-0.5,3.3));
#9492=CARTESIAN_POINT('',(-4.3,0.5,-3.3));
#9493=CARTESIAN_POINT('',(-4.3,0.5,-3.3));
#9494=CARTESIAN_POINT('',(-4.3,-0.5,-3.3));
#9495=CARTESIAN_POINT('Origin',(-3.3,-0.5,-4.3));
#9496=CARTESIAN_POINT('',(-3.3,-0.5,-4.3));
#9497=CARTESIAN_POINT('',(-3.3,-0.5,-4.3));
#9498=CARTESIAN_POINT('',(-3.3,0.5,-4.3));
#9499=CARTESIAN_POINT('',(-3.3,0.5,-4.3));
#9500=CARTESIAN_POINT('',(-3.3,-0.5,-4.3));
#9501=CARTESIAN_POINT('Origin',(3.3,-0.5,-4.3));
#9502=CARTESIAN_POINT('',(3.3,-0.5,-4.3));
#9503=CARTESIAN_POINT('',(3.3,-0.5,-4.3));
#9504=CARTESIAN_POINT('',(3.3,0.5,-4.3));
#9505=CARTESIAN_POINT('',(3.3,0.5,-4.3));
#9506=CARTESIAN_POINT('',(3.3,-0.5,-4.3));
#9507=CARTESIAN_POINT('Origin',(4.3,-0.5,-3.3));
#9508=CARTESIAN_POINT('',(4.3,-0.5,-3.3));
#9509=CARTESIAN_POINT('',(4.3,-0.5,-3.3));
#9510=CARTESIAN_POINT('',(4.3,0.5,-3.3));
#9511=CARTESIAN_POINT('',(4.3,0.5,-3.3));
#9512=CARTESIAN_POINT('',(4.3,-0.5,-3.3));
#9513=CARTESIAN_POINT('Origin',(4.3,-0.5,3.3));
#9514=CARTESIAN_POINT('',(4.3,-0.5,3.3));
#9515=CARTESIAN_POINT('',(4.3,-0.5,3.3));
#9516=CARTESIAN_POINT('',(4.3,0.5,3.3));
#9517=CARTESIAN_POINT('',(4.3,0.5,3.3));
#9518=CARTESIAN_POINT('',(4.3,-0.5,3.3));
#9519=CARTESIAN_POINT('Origin',(3.3,-0.5,4.3));
#9520=CARTESIAN_POINT('',(3.3,-0.5,4.3));
#9521=CARTESIAN_POINT('',(3.3,-0.5,4.3));
#9522=CARTESIAN_POINT('',(3.3,0.5,4.3));
#9523=CARTESIAN_POINT('',(3.3,0.5,4.3));
#9524=CARTESIAN_POINT('',(3.3,-0.5,4.3));
#9525=CARTESIAN_POINT('Origin',(-3.3,-0.5,4.3));
#9526=CARTESIAN_POINT('',(-3.3,-0.5,4.3));
#9527=CARTESIAN_POINT('',(-3.3,-0.5,4.3));
#9528=CARTESIAN_POINT('',(-3.3,0.5,4.3));
#9529=CARTESIAN_POINT('',(-3.3,0.5,4.3));
#9530=CARTESIAN_POINT('',(-3.3,-0.5,4.3));
#9531=CARTESIAN_POINT('Origin',(-4.3,-0.5,3.3));
#9532=CARTESIAN_POINT('',(-4.3,-0.5,3.3));
#9533=CARTESIAN_POINT('',(-4.3,0.5,3.3));
#9534=CARTESIAN_POINT('Origin',(0.,0.5,0.));
#9535=CARTESIAN_POINT('Origin',(0.,-0.5,0.));
#9536=CARTESIAN_POINT('',(0.,0.,0.));
#9537=CARTESIAN_POINT('Origin',(0.,0.,0.));
#9538=CARTESIAN_POINT('',(-1.8,-0.85,-2.20436423846524E-16));
#9539=CARTESIAN_POINT('Origin',(0.,-0.85,0.));
#9540=CARTESIAN_POINT('',(-1.8,0.85,-2.20436423846524E-16));
#9541=CARTESIAN_POINT('',(-1.8,0.,-2.20436423846524E-16));
#9542=CARTESIAN_POINT('Origin',(0.,0.85,0.));
#9543=CARTESIAN_POINT('Origin',(2.19089023002066,0.85,0.));
#9544=CARTESIAN_POINT('',(2.19089023002066,0.85,0.));
#9545=CARTESIAN_POINT('Origin',(0.,0.85,0.));
#9546=CARTESIAN_POINT('Origin',(3.99680288865056E-15,0.,0.));
#9547=CARTESIAN_POINT('',(3.85290688975075E-15,-1.76221774462768E-32,2.35));
#9548=CARTESIAN_POINT('',(3.85290688975075E-15,-1.76221774462768E-32,-2.35));
#9549=CARTESIAN_POINT('Origin',(3.99680288865056E-15,0.,0.));
#9550=CARTESIAN_POINT('',(2.19089023002066,-0.85,0.));
#9551=CARTESIAN_POINT('Origin',(0.,-0.85,0.));
#9552=CARTESIAN_POINT('Origin',(1.8,-0.85,0.));
#9553=CARTESIAN_POINT('Origin',(0.,1.55,0.));
#9554=CARTESIAN_POINT('',(1.42894191624432,1.8,0.825000000000001));
#9555=CARTESIAN_POINT('',(1.53744468918255,1.55,0.598968970568896));
#9556=CARTESIAN_POINT('Ctrl Pts',(1.42894191624432,1.8,0.825000000000001));
#9557=CARTESIAN_POINT('Ctrl Pts',(1.44466308895875,1.8,0.797770130104052));
#9558=CARTESIAN_POINT('Ctrl Pts',(1.46055812562105,1.79370633789704,0.768258557763732));
#9559=CARTESIAN_POINT('Ctrl Pts',(1.48824888379079,1.76817777258318,0.713138492740816));
#9560=CARTESIAN_POINT('Ctrl Pts',(1.50008999307766,1.74894552961493,0.687551581002689));
#9561=CARTESIAN_POINT('Ctrl Pts',(1.51812136280714,1.70460745840382,0.646764802471699));
#9562=CARTESIAN_POINT('Ctrl Pts',(1.52552758004446,1.67652816181843,0.628833667319578));
#9563=CARTESIAN_POINT('Ctrl Pts',(1.53516661651472,1.61494799959182,0.604921184808251));
#9564=CARTESIAN_POINT('Ctrl Pts',(1.53744468918255,1.58144291640553,0.598968970568896));
#9565=CARTESIAN_POINT('Ctrl Pts',(1.53744468918255,1.55,0.598968970568896));
#9566=CARTESIAN_POINT('',(1.42894191624432,1.3,0.825000000000001));
#9567=CARTESIAN_POINT('Ctrl Pts',(1.42894191624432,1.3,0.825000000000001));
#9568=CARTESIAN_POINT('Ctrl Pts',(1.4132207435299,1.3,0.852229869895949));
#9569=CARTESIAN_POINT('Ctrl Pts',(1.39561049050871,1.30629366210296,0.880751161609749));
#9570=CARTESIAN_POINT('Ctrl Pts',(1.36172049302549,1.33182222741682,0.932292094146256));
#9571=CARTESIAN_POINT('Ctrl Pts',(1.34548213209931,1.35105447038507,0.955340251466734));
#9572=CARTESIAN_POINT('Ctrl Pts',(1.31917543061769,1.39539254159618,0.99134926498299));
#9573=CARTESIAN_POINT('Ctrl Pts',(1.30734972067592,1.42347183818157,1.00672880483252));
#9574=CARTESIAN_POINT('Ctrl Pts',(1.29146042158868,1.48505200040818,1.02703269653942));
#9575=CARTESIAN_POINT('Ctrl Pts',(1.28744468918255,1.51855708359447,1.03198167246111));
#9576=CARTESIAN_POINT('Ctrl Pts',(1.28744468918255,1.58144291640553,1.03198167246111));
#9577=CARTESIAN_POINT('Ctrl Pts',(1.29146042158868,1.61494799959182,1.02703269653942));
#9578=CARTESIAN_POINT('Ctrl Pts',(1.30734972067592,1.67652816181843,1.00672880483252));
#9579=CARTESIAN_POINT('Ctrl Pts',(1.31917543061769,1.70460745840382,0.991349264982991));
#9580=CARTESIAN_POINT('Ctrl Pts',(1.34548213209931,1.74894552961493,0.955340251466735));
#9581=CARTESIAN_POINT('Ctrl Pts',(1.36172049302549,1.76817777258318,0.932292094146256));
#9582=CARTESIAN_POINT('Ctrl Pts',(1.39561049050871,1.79370633789704,0.880751161609749));
#9583=CARTESIAN_POINT('Ctrl Pts',(1.4132207435299,1.8,0.85222986989595));
#9584=CARTESIAN_POINT('Ctrl Pts',(1.42894191624432,1.8,0.825000000000001));
#9585=CARTESIAN_POINT('Ctrl Pts',(1.53744468918255,1.55,0.598968970568896));
#9586=CARTESIAN_POINT('Ctrl Pts',(1.53744468918255,1.51855708359447,0.598968970568896));
#9587=CARTESIAN_POINT('Ctrl Pts',(1.53516661651472,1.48505200040818,0.60492118480825));
#9588=CARTESIAN_POINT('Ctrl Pts',(1.52552758004446,1.42347183818157,0.628833667319578));
#9589=CARTESIAN_POINT('Ctrl Pts',(1.51812136280714,1.39539254159618,0.646764802471699));
#9590=CARTESIAN_POINT('Ctrl Pts',(1.50008999307766,1.35105447038507,0.687551581002689));
#9591=CARTESIAN_POINT('Ctrl Pts',(1.48824888379079,1.33182222741682,0.713138492740816));
#9592=CARTESIAN_POINT('Ctrl Pts',(1.46055812562105,1.30629366210296,0.768258557763732));
#9593=CARTESIAN_POINT('Ctrl Pts',(1.44466308895875,1.3,0.797770130104052));
#9594=CARTESIAN_POINT('Ctrl Pts',(1.42894191624432,1.3,0.825000000000001));
#9595=CARTESIAN_POINT('',(0.963525491562421,1.55,0.267616567329818));
#9596=CARTESIAN_POINT('',(0.125,1.55,-0.21650635094611));
#9597=CARTESIAN_POINT('Ctrl Pts',(0.963525491562421,1.55,0.267616567329818));
#9598=CARTESIAN_POINT('Ctrl Pts',(0.963525491562421,1.5815373526696,0.267616567329818));
#9599=CARTESIAN_POINT('Ctrl Pts',(0.961833761492987,1.61508042700263,0.273949373987484));
#9600=CARTESIAN_POINT('Ctrl Pts',(0.954308486908894,1.67663267125761,0.299111603474268));
#9601=CARTESIAN_POINT('Ctrl Pts',(0.948394987258249,1.70465411363682,0.31788699900678));
#9602=CARTESIAN_POINT('Ctrl Pts',(0.933155485613026,1.74889618382539,0.360174810895352));
#9603=CARTESIAN_POINT('Ctrl Pts',(0.92278792026947,1.76811531482682,0.386546956384144));
#9604=CARTESIAN_POINT('Ctrl Pts',(0.897143218189782,1.79367084275751,0.442820664919227));
#9605=CARTESIAN_POINT('Ctrl Pts',(0.881791875377343,1.8,0.472691670144998));
#9606=CARTESIAN_POINT('Ctrl Pts',(0.850258932191534,1.8,0.527308329855003));
#9607=CARTESIAN_POINT('Ctrl Pts',(0.832065554235658,1.79367084275751,0.555538485325664));
#9608=CARTESIAN_POINT('Ctrl Pts',(0.796153444118959,1.76811531482682,0.605884303066698));
#9609=CARTESIAN_POINT('Ctrl Pts',(0.778498278845144,1.74889618382539,0.62804895077401));
#9610=CARTESIAN_POINT('Ctrl Pts',(0.749495710301794,1.70465411363682,0.662390652284073));
#9611=CARTESIAN_POINT('Ctrl Pts',(0.73619249062986,1.67663267125761,0.676899590973058));
#9612=CARTESIAN_POINT('Ctrl Pts',(0.718163997970498,1.61508042700263,0.695997784676728));
#9613=CARTESIAN_POINT('Ctrl Pts',(0.713525491562421,1.5815373526696,0.700629269222037));
#9614=CARTESIAN_POINT('Ctrl Pts',(0.713525491562421,1.5184626473304,0.700629269222037));
#9615=CARTESIAN_POINT('Ctrl Pts',(0.718163997970498,1.48491957299737,0.695997784676728));
#9616=CARTESIAN_POINT('Ctrl Pts',(0.73619249062986,1.42336732874239,0.676899590973058));
#9617=CARTESIAN_POINT('Ctrl Pts',(0.749495710301794,1.39534588636318,0.662390652284073));
#9618=CARTESIAN_POINT('Ctrl Pts',(0.778498278845144,1.35110381617461,0.62804895077401));
#9619=CARTESIAN_POINT('Ctrl Pts',(0.796153444118959,1.33188468517318,0.605884303066698));
#9620=CARTESIAN_POINT('Ctrl Pts',(0.832065554235658,1.30632915724249,0.555538485325664));
#9621=CARTESIAN_POINT('Ctrl Pts',(0.850258932191534,1.3,0.527308329855003));
#9622=CARTESIAN_POINT('Ctrl Pts',(0.881791875377343,1.3,0.472691670144998));
#9623=CARTESIAN_POINT('Ctrl Pts',(0.897143218189782,1.30632915724249,0.442820664919227));
#9624=CARTESIAN_POINT('Ctrl Pts',(0.92278792026947,1.33188468517318,0.386546956384144));
#9625=CARTESIAN_POINT('Ctrl Pts',(0.933155485613026,1.35110381617461,0.360174810895352));
#9626=CARTESIAN_POINT('Ctrl Pts',(0.948394987258249,1.39534588636318,0.31788699900678));
#9627=CARTESIAN_POINT('Ctrl Pts',(0.954308486908894,1.42336732874239,0.299111603474268));
#9628=CARTESIAN_POINT('Ctrl Pts',(0.961833761492987,1.48491957299738,0.273949373987484));
#9629=CARTESIAN_POINT('Ctrl Pts',(0.963525491562421,1.5184626473304,0.267616567329818));
#9630=CARTESIAN_POINT('Ctrl Pts',(0.963525491562421,1.55,0.267616567329818));
#9631=CARTESIAN_POINT('Origin',(0.,1.55,0.));
#9632=CARTESIAN_POINT('',(-0.713525491562421,1.55,-0.700629269222037));
#9633=CARTESIAN_POINT('Ctrl Pts',(-0.713525491562421,1.55,-0.700629269222037));
#9634=CARTESIAN_POINT('Ctrl Pts',(-0.713525491562421,1.5184626473304,-0.700629269222037));
#9635=CARTESIAN_POINT('Ctrl Pts',(-0.718163997970498,1.48491957299737,-0.695997784676728));
#9636=CARTESIAN_POINT('Ctrl Pts',(-0.73619249062986,1.42336732874239,-0.676899590973058));
#9637=CARTESIAN_POINT('Ctrl Pts',(-0.749495710301794,1.39534588636318,-0.662390652284073));
#9638=CARTESIAN_POINT('Ctrl Pts',(-0.778498278845144,1.35110381617461,-0.62804895077401));
#9639=CARTESIAN_POINT('Ctrl Pts',(-0.796153444118959,1.33188468517318,-0.605884303066698));
#9640=CARTESIAN_POINT('Ctrl Pts',(-0.832065554235658,1.30632915724249,-0.555538485325664));
#9641=CARTESIAN_POINT('Ctrl Pts',(-0.850258932191534,1.3,-0.527308329855003));
#9642=CARTESIAN_POINT('Ctrl Pts',(-0.881791875377343,1.3,-0.472691670144998));
#9643=CARTESIAN_POINT('Ctrl Pts',(-0.897143218189782,1.30632915724249,-0.442820664919227));
#9644=CARTESIAN_POINT('Ctrl Pts',(-0.92278792026947,1.33188468517318,-0.386546956384144));
#9645=CARTESIAN_POINT('Ctrl Pts',(-0.933155485613026,1.35110381617461,-0.360174810895352));
#9646=CARTESIAN_POINT('Ctrl Pts',(-0.948394987258249,1.39534588636318,-0.31788699900678));
#9647=CARTESIAN_POINT('Ctrl Pts',(-0.954308486908894,1.42336732874239,-0.299111603474268));
#9648=CARTESIAN_POINT('Ctrl Pts',(-0.961833761492986,1.48491957299737,-0.273949373987484));
#9649=CARTESIAN_POINT('Ctrl Pts',(-0.963525491562421,1.5184626473304,-0.267616567329818));
#9650=CARTESIAN_POINT('Ctrl Pts',(-0.963525491562421,1.5815373526696,-0.267616567329818));
#9651=CARTESIAN_POINT('Ctrl Pts',(-0.961833761492986,1.61508042700263,-0.273949373987484));
#9652=CARTESIAN_POINT('Ctrl Pts',(-0.954308486908894,1.67663267125761,-0.299111603474268));
#9653=CARTESIAN_POINT('Ctrl Pts',(-0.948394987258249,1.70465411363682,-0.31788699900678));
#9654=CARTESIAN_POINT('Ctrl Pts',(-0.933155485613026,1.74889618382539,-0.360174810895352));
#9655=CARTESIAN_POINT('Ctrl Pts',(-0.92278792026947,1.76811531482682,-0.386546956384144));
#9656=CARTESIAN_POINT('Ctrl Pts',(-0.897143218189782,1.79367084275751,-0.442820664919227));
#9657=CARTESIAN_POINT('Ctrl Pts',(-0.881791875377343,1.8,-0.472691670144998));
#9658=CARTESIAN_POINT('Ctrl Pts',(-0.850258932191534,1.8,-0.527308329855003));
#9659=CARTESIAN_POINT('Ctrl Pts',(-0.832065554235658,1.79367084275751,-0.555538485325664));
#9660=CARTESIAN_POINT('Ctrl Pts',(-0.796153444118959,1.76811531482682,-0.605884303066698));
#9661=CARTESIAN_POINT('Ctrl Pts',(-0.778498278845144,1.74889618382539,-0.62804895077401));
#9662=CARTESIAN_POINT('Ctrl Pts',(-0.749495710301794,1.70465411363682,-0.662390652284073));
#9663=CARTESIAN_POINT('Ctrl Pts',(-0.73619249062986,1.67663267125761,-0.676899590973058));
#9664=CARTESIAN_POINT('Ctrl Pts',(-0.718163997970498,1.61508042700263,-0.695997784676728));
#9665=CARTESIAN_POINT('Ctrl Pts',(-0.713525491562421,1.5815373526696,-0.700629269222037));
#9666=CARTESIAN_POINT('Ctrl Pts',(-0.713525491562421,1.55,-0.700629269222037));
#9667=CARTESIAN_POINT('',(-1.28744468918255,1.55,-1.03198167246111));
#9668=CARTESIAN_POINT('',(0.125,1.55,-0.21650635094611));
#9669=CARTESIAN_POINT('',(-1.42894191624432,1.3,-0.825000000000001));
#9670=CARTESIAN_POINT('Ctrl Pts',(-1.42894191624432,1.3,-0.825000000000001));
#9671=CARTESIAN_POINT('Ctrl Pts',(-1.4132207435299,1.3,-0.852229869895949));
#9672=CARTESIAN_POINT('Ctrl Pts',(-1.39561049050871,1.30629366210296,-0.880751161609749));
#9673=CARTESIAN_POINT('Ctrl Pts',(-1.36172049302549,1.33182222741682,-0.932292094146256));
#9674=CARTESIAN_POINT('Ctrl Pts',(-1.34548213209931,1.35105447038507,-0.955340251466735));
#9675=CARTESIAN_POINT('Ctrl Pts',(-1.31917543061769,1.39539254159618,-0.991349264982991));
#9676=CARTESIAN_POINT('Ctrl Pts',(-1.30734972067592,1.42347183818157,-1.00672880483252));
#9677=CARTESIAN_POINT('Ctrl Pts',(-1.29146042158868,1.48505200040818,-1.02703269653942));
#9678=CARTESIAN_POINT('Ctrl Pts',(-1.28744468918255,1.51855708359447,-1.03198167246111));
#9679=CARTESIAN_POINT('Ctrl Pts',(-1.28744468918255,1.55,-1.03198167246111));
#9680=CARTESIAN_POINT('',(-1.42894191624432,1.8,-0.825000000000001));
#9681=CARTESIAN_POINT('Ctrl Pts',(-1.42894191624432,1.8,-0.825000000000001));
#9682=CARTESIAN_POINT('Ctrl Pts',(-1.44466308895875,1.8,-0.797770130104052));
#9683=CARTESIAN_POINT('Ctrl Pts',(-1.46055812562105,1.79370633789704,-0.768258557763732));
#9684=CARTESIAN_POINT('Ctrl Pts',(-1.48824888379079,1.76817777258318,-0.713138492740816));
#9685=CARTESIAN_POINT('Ctrl Pts',(-1.50008999307766,1.74894552961493,-0.687551581002689));
#9686=CARTESIAN_POINT('Ctrl Pts',(-1.51812136280714,1.70460745840382,-0.646764802471699));
#9687=CARTESIAN_POINT('Ctrl Pts',(-1.52552758004446,1.67652816181843,-0.628833667319578));
#9688=CARTESIAN_POINT('Ctrl Pts',(-1.53516661651472,1.61494799959182,-0.60492118480825));
#9689=CARTESIAN_POINT('Ctrl Pts',(-1.53744468918255,1.58144291640553,-0.598968970568896));
#9690=CARTESIAN_POINT('Ctrl Pts',(-1.53744468918255,1.51855708359447,-0.598968970568896));
#9691=CARTESIAN_POINT('Ctrl Pts',(-1.53516661651472,1.48505200040818,-0.60492118480825));
#9692=CARTESIAN_POINT('Ctrl Pts',(-1.52552758004446,1.42347183818157,-0.628833667319578));
#9693=CARTESIAN_POINT('Ctrl Pts',(-1.51812136280714,1.39539254159618,-0.646764802471699));
#9694=CARTESIAN_POINT('Ctrl Pts',(-1.50008999307766,1.35105447038507,-0.687551581002689));
#9695=CARTESIAN_POINT('Ctrl Pts',(-1.48824888379079,1.33182222741682,-0.713138492740816));
#9696=CARTESIAN_POINT('Ctrl Pts',(-1.46055812562105,1.30629366210296,-0.768258557763732));
#9697=CARTESIAN_POINT('Ctrl Pts',(-1.44466308895875,1.3,-0.797770130104052));
#9698=CARTESIAN_POINT('Ctrl Pts',(-1.42894191624432,1.3,-0.825000000000001));
#9699=CARTESIAN_POINT('Ctrl Pts',(-1.28744468918255,1.55,-1.03198167246111));
#9700=CARTESIAN_POINT('Ctrl Pts',(-1.28744468918255,1.58144291640553,-1.03198167246111));
#9701=CARTESIAN_POINT('Ctrl Pts',(-1.29146042158868,1.61494799959182,-1.02703269653942));
#9702=CARTESIAN_POINT('Ctrl Pts',(-1.30734972067592,1.67652816181843,-1.00672880483252));
#9703=CARTESIAN_POINT('Ctrl Pts',(-1.31917543061769,1.70460745840382,-0.991349264982991));
#9704=CARTESIAN_POINT('Ctrl Pts',(-1.34548213209931,1.74894552961493,-0.955340251466734));
#9705=CARTESIAN_POINT('Ctrl Pts',(-1.36172049302549,1.76817777258318,-0.932292094146256));
#9706=CARTESIAN_POINT('Ctrl Pts',(-1.39561049050871,1.79370633789704,-0.880751161609749));
#9707=CARTESIAN_POINT('Ctrl Pts',(-1.4132207435299,1.8,-0.852229869895949));
#9708=CARTESIAN_POINT('Ctrl Pts',(-1.42894191624432,1.8,-0.825000000000001));
#9709=CARTESIAN_POINT('Origin',(0.,1.55,0.));
#9710=CARTESIAN_POINT('',(-1.65,0.85,-2.02066721859313E-16));
#9711=CARTESIAN_POINT('Origin',(0.,0.85,0.));
#9712=CARTESIAN_POINT('',(-1.65,2.25,-2.02066721859313E-16));
#9713=CARTESIAN_POINT('',(-1.65,1.55,-2.02066721859313E-16));
#9714=CARTESIAN_POINT('Origin',(0.,2.25,0.));
#9715=CARTESIAN_POINT('',(-1.42894191624432,1.3,0.825));
#9716=CARTESIAN_POINT('',(-1.42894191624432,1.8,0.825));
#9717=CARTESIAN_POINT('Ctrl Pts',(-1.42894191624432,1.3,0.825));
#9718=CARTESIAN_POINT('Ctrl Pts',(-1.44466308895875,1.3,0.797770130104051));
#9719=CARTESIAN_POINT('Ctrl Pts',(-1.46055812562105,1.30629366210296,0.768258557763731));
#9720=CARTESIAN_POINT('Ctrl Pts',(-1.48824888379079,1.33182222741682,0.713138492740815));
#9721=CARTESIAN_POINT('Ctrl Pts',(-1.50008999307766,1.35105447038507,0.687551581002688));
#9722=CARTESIAN_POINT('Ctrl Pts',(-1.51812136280714,1.39539254159618,0.646764802471698));
#9723=CARTESIAN_POINT('Ctrl Pts',(-1.52552758004446,1.42347183818157,0.628833667319577));
#9724=CARTESIAN_POINT('Ctrl Pts',(-1.53516661651472,1.48505200040818,0.604921184808249));
#9725=CARTESIAN_POINT('Ctrl Pts',(-1.53744468918255,1.51855708359447,0.598968970568895));
#9726=CARTESIAN_POINT('Ctrl Pts',(-1.53744468918255,1.58144291640553,0.598968970568895));
#9727=CARTESIAN_POINT('Ctrl Pts',(-1.53516661651472,1.61494799959182,0.604921184808249));
#9728=CARTESIAN_POINT('Ctrl Pts',(-1.52552758004446,1.67652816181843,0.628833667319577));
#9729=CARTESIAN_POINT('Ctrl Pts',(-1.51812136280714,1.70460745840382,0.646764802471698));
#9730=CARTESIAN_POINT('Ctrl Pts',(-1.50008999307766,1.74894552961493,0.687551581002688));
#9731=CARTESIAN_POINT('Ctrl Pts',(-1.48824888379079,1.76817777258318,0.713138492740815));
#9732=CARTESIAN_POINT('Ctrl Pts',(-1.46055812562105,1.79370633789704,0.768258557763731));
#9733=CARTESIAN_POINT('Ctrl Pts',(-1.44466308895875,1.8,0.797770130104051));
#9734=CARTESIAN_POINT('Ctrl Pts',(-1.42894191624432,1.8,0.825));
#9735=CARTESIAN_POINT('',(-1.28744468918255,1.55,1.03198167246111));
#9736=CARTESIAN_POINT('Ctrl Pts',(-1.42894191624432,1.8,0.825));
#9737=CARTESIAN_POINT('Ctrl Pts',(-1.4132207435299,1.8,0.852229869895948));
#9738=CARTESIAN_POINT('Ctrl Pts',(-1.39561049050871,1.79370633789704,0.880751161609747));
#9739=CARTESIAN_POINT('Ctrl Pts',(-1.36172049302549,1.76817777258318,0.932292094146255));
#9740=CARTESIAN_POINT('Ctrl Pts',(-1.34548213209931,1.74894552961493,0.955340251466733));
#9741=CARTESIAN_POINT('Ctrl Pts',(-1.31917543061769,1.70460745840382,0.991349264982989));
#9742=CARTESIAN_POINT('Ctrl Pts',(-1.30734972067592,1.67652816181843,1.00672880483252));
#9743=CARTESIAN_POINT('Ctrl Pts',(-1.29146042158868,1.61494799959182,1.02703269653942));
#9744=CARTESIAN_POINT('Ctrl Pts',(-1.28744468918255,1.58144291640553,1.03198167246111));
#9745=CARTESIAN_POINT('Ctrl Pts',(-1.28744468918255,1.55,1.03198167246111));
#9746=CARTESIAN_POINT('Ctrl Pts',(-1.28744468918255,1.55,1.03198167246111));
#9747=CARTESIAN_POINT('Ctrl Pts',(-1.28744468918255,1.51855708359447,1.03198167246111));
#9748=CARTESIAN_POINT('Ctrl Pts',(-1.29146042158868,1.48505200040818,1.02703269653942));
#9749=CARTESIAN_POINT('Ctrl Pts',(-1.30734972067592,1.42347183818157,1.00672880483252));
#9750=CARTESIAN_POINT('Ctrl Pts',(-1.31917543061769,1.39539254159618,0.99134926498299));
#9751=CARTESIAN_POINT('Ctrl Pts',(-1.34548213209931,1.35105447038508,0.955340251466733));
#9752=CARTESIAN_POINT('Ctrl Pts',(-1.36172049302549,1.33182222741682,0.932292094146255));
#9753=CARTESIAN_POINT('Ctrl Pts',(-1.39561049050871,1.30629366210296,0.880751161609748));
#9754=CARTESIAN_POINT('Ctrl Pts',(-1.4132207435299,1.3,0.852229869895949));
#9755=CARTESIAN_POINT('Ctrl Pts',(-1.42894191624432,1.3,0.825));
#9756=CARTESIAN_POINT('',(1.42894191624432,1.8,-0.825));
#9757=CARTESIAN_POINT('',(1.42894191624432,1.3,-0.825));
#9758=CARTESIAN_POINT('Ctrl Pts',(1.42894191624432,1.8,-0.825));
#9759=CARTESIAN_POINT('Ctrl Pts',(1.4132207435299,1.8,-0.852229869895949));
#9760=CARTESIAN_POINT('Ctrl Pts',(1.39561049050871,1.79370633789704,-0.880751161609748));
#9761=CARTESIAN_POINT('Ctrl Pts',(1.36172049302549,1.76817777258318,-0.932292094146255));
#9762=CARTESIAN_POINT('Ctrl Pts',(1.34548213209931,1.74894552961493,-0.955340251466734));
#9763=CARTESIAN_POINT('Ctrl Pts',(1.31917543061769,1.70460745840382,-0.99134926498299));
#9764=CARTESIAN_POINT('Ctrl Pts',(1.30734972067592,1.67652816181843,-1.00672880483252));
#9765=CARTESIAN_POINT('Ctrl Pts',(1.29146042158868,1.61494799959182,-1.02703269653942));
#9766=CARTESIAN_POINT('Ctrl Pts',(1.28744468918255,1.58144291640553,-1.03198167246111));
#9767=CARTESIAN_POINT('Ctrl Pts',(1.28744468918255,1.51855708359447,-1.03198167246111));
#9768=CARTESIAN_POINT('Ctrl Pts',(1.29146042158868,1.48505200040818,-1.02703269653942));
#9769=CARTESIAN_POINT('Ctrl Pts',(1.30734972067592,1.42347183818157,-1.00672880483252));
#9770=CARTESIAN_POINT('Ctrl Pts',(1.31917543061769,1.39539254159618,-0.99134926498299));
#9771=CARTESIAN_POINT('Ctrl Pts',(1.34548213209931,1.35105447038507,-0.955340251466734));
#9772=CARTESIAN_POINT('Ctrl Pts',(1.36172049302549,1.33182222741682,-0.932292094146255));
#9773=CARTESIAN_POINT('Ctrl Pts',(1.39561049050871,1.30629366210296,-0.880751161609748));
#9774=CARTESIAN_POINT('Ctrl Pts',(1.4132207435299,1.3,-0.852229869895948));
#9775=CARTESIAN_POINT('Ctrl Pts',(1.42894191624432,1.3,-0.825));
#9776=CARTESIAN_POINT('',(1.53744468918255,1.55,-0.598968970568895));
#9777=CARTESIAN_POINT('Ctrl Pts',(1.42894191624432,1.3,-0.825));
#9778=CARTESIAN_POINT('Ctrl Pts',(1.44466308895875,1.3,-0.797770130104051));
#9779=CARTESIAN_POINT('Ctrl Pts',(1.46055812562105,1.30629366210296,-0.768258557763731));
#9780=CARTESIAN_POINT('Ctrl Pts',(1.48824888379079,1.33182222741682,-0.713138492740815));
#9781=CARTESIAN_POINT('Ctrl Pts',(1.50008999307766,1.35105447038507,-0.687551581002688));
#9782=CARTESIAN_POINT('Ctrl Pts',(1.51812136280714,1.39539254159618,-0.646764802471698));
#9783=CARTESIAN_POINT('Ctrl Pts',(1.52552758004446,1.42347183818157,-0.628833667319577));
#9784=CARTESIAN_POINT('Ctrl Pts',(1.53516661651472,1.48505200040818,-0.604921184808249));
#9785=CARTESIAN_POINT('Ctrl Pts',(1.53744468918255,1.51855708359447,-0.598968970568895));
#9786=CARTESIAN_POINT('Ctrl Pts',(1.53744468918255,1.55,-0.598968970568895));
#9787=CARTESIAN_POINT('Ctrl Pts',(1.53744468918255,1.55,-0.598968970568895));
#9788=CARTESIAN_POINT('Ctrl Pts',(1.53744468918255,1.58144291640553,-0.598968970568895));
#9789=CARTESIAN_POINT('Ctrl Pts',(1.53516661651472,1.61494799959182,-0.604921184808249));
#9790=CARTESIAN_POINT('Ctrl Pts',(1.52552758004446,1.67652816181843,-0.628833667319577));
#9791=CARTESIAN_POINT('Ctrl Pts',(1.51812136280714,1.70460745840382,-0.646764802471698));
#9792=CARTESIAN_POINT('Ctrl Pts',(1.50008999307766,1.74894552961493,-0.687551581002688));
#9793=CARTESIAN_POINT('Ctrl Pts',(1.48824888379079,1.76817777258318,-0.713138492740815));
#9794=CARTESIAN_POINT('Ctrl Pts',(1.46055812562105,1.79370633789704,-0.768258557763731));
#9795=CARTESIAN_POINT('Ctrl Pts',(1.44466308895875,1.8,-0.797770130104051));
#9796=CARTESIAN_POINT('Ctrl Pts',(1.42894191624432,1.8,-0.825));
#9797=CARTESIAN_POINT('',(0.,1.3,-1.65));
#9798=CARTESIAN_POINT('',(0.,1.8,-1.65));
#9799=CARTESIAN_POINT('Ctrl Pts',(1.38777878078145E-17,1.3,-1.65));
#9800=CARTESIAN_POINT('Ctrl Pts',(0.0314423454288489,1.3,-1.65));
#9801=CARTESIAN_POINT('Ctrl Pts',(0.0649476351123396,1.30629366210296,-1.64900971937348));
#9802=CARTESIAN_POINT('Ctrl Pts',(0.126528390765307,1.33182222741682,-1.64543058688707));
#9803=CARTESIAN_POINT('Ctrl Pts',(0.154607860978348,1.35105447038507,-1.64289183246942));
#9804=CARTESIAN_POINT('Ctrl Pts',(0.198945932189457,1.39539254159618,-1.63811406745469));
#9805=CARTESIAN_POINT('Ctrl Pts',(0.218177859368546,1.42347183818157,-1.63556247215209));
#9806=CARTESIAN_POINT('Ctrl Pts',(0.243706194926033,1.48505200040818,-1.63195388134767));
#9807=CARTESIAN_POINT('Ctrl Pts',(0.25,1.51855708359447,-1.63095064303001));
#9808=CARTESIAN_POINT('Ctrl Pts',(0.25,1.58144291640553,-1.63095064303001));
#9809=CARTESIAN_POINT('Ctrl Pts',(0.243706194926033,1.61494799959182,-1.63195388134767));
#9810=CARTESIAN_POINT('Ctrl Pts',(0.218177859368546,1.67652816181843,-1.63556247215209));
#9811=CARTESIAN_POINT('Ctrl Pts',(0.198945932189457,1.70460745840382,-1.63811406745469));
#9812=CARTESIAN_POINT('Ctrl Pts',(0.154607860978349,1.74894552961493,-1.64289183246942));
#9813=CARTESIAN_POINT('Ctrl Pts',(0.126528390765307,1.76817777258318,-1.64543058688707));
#9814=CARTESIAN_POINT('Ctrl Pts',(0.0649476351123398,1.79370633789704,-1.64900971937348));
#9815=CARTESIAN_POINT('Ctrl Pts',(0.031442345428849,1.8,-1.65));
#9816=CARTESIAN_POINT('Ctrl Pts',(7.63278329429795E-17,1.8,-1.65));
#9817=CARTESIAN_POINT('',(-0.25,1.55,-1.63095064303001));
#9818=CARTESIAN_POINT('Ctrl Pts',(9.0205620750794E-17,1.8,-1.65));
#9819=CARTESIAN_POINT('Ctrl Pts',(-0.0314423454288488,1.8,-1.65));
#9820=CARTESIAN_POINT('Ctrl Pts',(-0.0649476351123396,1.79370633789704,
-1.64900971937348));
#9821=CARTESIAN_POINT('Ctrl Pts',(-0.126528390765307,1.76817777258318,-1.64543058688707));
#9822=CARTESIAN_POINT('Ctrl Pts',(-0.154607860978348,1.74894552961493,-1.64289183246942));
#9823=CARTESIAN_POINT('Ctrl Pts',(-0.198945932189456,1.70460745840382,-1.63811406745469));
#9824=CARTESIAN_POINT('Ctrl Pts',(-0.218177859368546,1.67652816181843,-1.63556247215209));
#9825=CARTESIAN_POINT('Ctrl Pts',(-0.243706194926033,1.61494799959182,-1.63195388134767));
#9826=CARTESIAN_POINT('Ctrl Pts',(-0.25,1.58144291640553,-1.63095064303001));
#9827=CARTESIAN_POINT('Ctrl Pts',(-0.25,1.55,-1.63095064303001));
#9828=CARTESIAN_POINT('Ctrl Pts',(-0.25,1.55,-1.63095064303001));
#9829=CARTESIAN_POINT('Ctrl Pts',(-0.25,1.51855708359447,-1.63095064303001));
#9830=CARTESIAN_POINT('Ctrl Pts',(-0.243706194926033,1.48505200040818,-1.63195388134767));
#9831=CARTESIAN_POINT('Ctrl Pts',(-0.218177859368546,1.42347183818157,-1.63556247215209));
#9832=CARTESIAN_POINT('Ctrl Pts',(-0.198945932189457,1.39539254159618,-1.63811406745469));
#9833=CARTESIAN_POINT('Ctrl Pts',(-0.154607860978349,1.35105447038507,-1.64289183246942));
#9834=CARTESIAN_POINT('Ctrl Pts',(-0.126528390765307,1.33182222741682,-1.64543058688707));
#9835=CARTESIAN_POINT('Ctrl Pts',(-0.0649476351123398,1.30629366210296,
-1.64900971937348));
#9836=CARTESIAN_POINT('Ctrl Pts',(-0.031442345428849,1.3,-1.65));
#9837=CARTESIAN_POINT('Ctrl Pts',(-4.85722573273506E-17,1.3,-1.65));
#9838=CARTESIAN_POINT('',(0.,1.8,1.65));
#9839=CARTESIAN_POINT('',(0.,1.3,1.65));
#9840=CARTESIAN_POINT('Ctrl Pts',(8.32667268468867E-17,1.8,1.65));
#9841=CARTESIAN_POINT('Ctrl Pts',(0.031442345428849,1.8,1.65));
#9842=CARTESIAN_POINT('Ctrl Pts',(0.0649476351123398,1.79370633789704,1.64900971937348));
#9843=CARTESIAN_POINT('Ctrl Pts',(0.126528390765307,1.76817777258318,1.64543058688707));
#9844=CARTESIAN_POINT('Ctrl Pts',(0.154607860978349,1.74894552961493,1.64289183246942));
#9845=CARTESIAN_POINT('Ctrl Pts',(0.198945932189457,1.70460745840382,1.63811406745469));
#9846=CARTESIAN_POINT('Ctrl Pts',(0.218177859368546,1.67652816181843,1.63556247215209));
#9847=CARTESIAN_POINT('Ctrl Pts',(0.243706194926033,1.61494799959182,1.63195388134767));
#9848=CARTESIAN_POINT('Ctrl Pts',(0.25,1.58144291640553,1.63095064303001));
#9849=CARTESIAN_POINT('Ctrl Pts',(0.25,1.51855708359447,1.63095064303001));
#9850=CARTESIAN_POINT('Ctrl Pts',(0.243706194926033,1.48505200040818,1.63195388134767));
#9851=CARTESIAN_POINT('Ctrl Pts',(0.218177859368546,1.42347183818157,1.63556247215209));
#9852=CARTESIAN_POINT('Ctrl Pts',(0.198945932189457,1.39539254159618,1.63811406745469));
#9853=CARTESIAN_POINT('Ctrl Pts',(0.154607860978348,1.35105447038507,1.64289183246942));
#9854=CARTESIAN_POINT('Ctrl Pts',(0.126528390765307,1.33182222741682,1.64543058688707));
#9855=CARTESIAN_POINT('Ctrl Pts',(0.0649476351123397,1.30629366210296,1.64900971937348));
#9856=CARTESIAN_POINT('Ctrl Pts',(0.0314423454288488,1.3,1.65));
#9857=CARTESIAN_POINT('Ctrl Pts',(-1.38777878078145E-17,1.3,1.65));
#9858=CARTESIAN_POINT('',(-0.25,1.55,1.63095064303001));
#9859=CARTESIAN_POINT('Ctrl Pts',(-5.55111512312578E-17,1.3,1.65));
#9860=CARTESIAN_POINT('Ctrl Pts',(-0.031442345428849,1.3,1.65));
#9861=CARTESIAN_POINT('Ctrl Pts',(-0.0649476351123398,1.30629366210296,
1.64900971937348));
#9862=CARTESIAN_POINT('Ctrl Pts',(-0.126528390765307,1.33182222741682,1.64543058688707));
#9863=CARTESIAN_POINT('Ctrl Pts',(-0.154607860978349,1.35105447038507,1.64289183246942));
#9864=CARTESIAN_POINT('Ctrl Pts',(-0.198945932189457,1.39539254159618,1.63811406745469));
#9865=CARTESIAN_POINT('Ctrl Pts',(-0.218177859368546,1.42347183818157,1.63556247215209));
#9866=CARTESIAN_POINT('Ctrl Pts',(-0.243706194926033,1.48505200040818,1.63195388134767));
#9867=CARTESIAN_POINT('Ctrl Pts',(-0.25,1.51855708359447,1.63095064303001));
#9868=CARTESIAN_POINT('Ctrl Pts',(-0.25,1.55,1.63095064303001));
#9869=CARTESIAN_POINT('Ctrl Pts',(-0.25,1.55,1.63095064303001));
#9870=CARTESIAN_POINT('Ctrl Pts',(-0.25,1.58144291640553,1.63095064303001));
#9871=CARTESIAN_POINT('Ctrl Pts',(-0.243706194926033,1.61494799959182,1.63195388134767));
#9872=CARTESIAN_POINT('Ctrl Pts',(-0.218177859368546,1.67652816181843,1.63556247215209));
#9873=CARTESIAN_POINT('Ctrl Pts',(-0.198945932189456,1.70460745840382,1.63811406745469));
#9874=CARTESIAN_POINT('Ctrl Pts',(-0.154607860978348,1.74894552961493,1.64289183246942));
#9875=CARTESIAN_POINT('Ctrl Pts',(-0.126528390765307,1.76817777258318,1.64543058688707));
#9876=CARTESIAN_POINT('Ctrl Pts',(-0.0649476351123396,1.79370633789704,
1.64900971937348));
#9877=CARTESIAN_POINT('Ctrl Pts',(-0.0314423454288488,1.8,1.65));
#9878=CARTESIAN_POINT('Ctrl Pts',(7.63278329429795E-17,1.8,1.65));
#9879=CARTESIAN_POINT('Origin',(0.,1.55,0.));
#9880=CARTESIAN_POINT('',(-0.713525491562421,1.55,0.700629269222037));
#9881=CARTESIAN_POINT('',(0.125,1.55,0.21650635094611));
#9882=CARTESIAN_POINT('Ctrl Pts',(-0.713525491562421,1.55,0.700629269222037));
#9883=CARTESIAN_POINT('Ctrl Pts',(-0.713525491562421,1.5815373526696,0.700629269222037));
#9884=CARTESIAN_POINT('Ctrl Pts',(-0.718163997970498,1.61508042700263,0.695997784676727));
#9885=CARTESIAN_POINT('Ctrl Pts',(-0.73619249062986,1.67663267125761,0.676899590973058));
#9886=CARTESIAN_POINT('Ctrl Pts',(-0.749495710301795,1.70465411363682,0.662390652284073));
#9887=CARTESIAN_POINT('Ctrl Pts',(-0.778498278845144,1.74889618382539,0.628048950774009));
#9888=CARTESIAN_POINT('Ctrl Pts',(-0.796153444118959,1.76811531482682,0.605884303066698));
#9889=CARTESIAN_POINT('Ctrl Pts',(-0.832065554235658,1.79367084275751,0.555538485325663));
#9890=CARTESIAN_POINT('Ctrl Pts',(-0.850258932191534,1.8,0.527308329855002));
#9891=CARTESIAN_POINT('Ctrl Pts',(-0.881791875377343,1.8,0.472691670144998));
#9892=CARTESIAN_POINT('Ctrl Pts',(-0.897143218189782,1.79367084275751,0.442820664919227));
#9893=CARTESIAN_POINT('Ctrl Pts',(-0.92278792026947,1.76811531482682,0.386546956384144));
#9894=CARTESIAN_POINT('Ctrl Pts',(-0.933155485613026,1.74889618382539,0.360174810895352));
#9895=CARTESIAN_POINT('Ctrl Pts',(-0.948394987258249,1.70465411363682,0.31788699900678));
#9896=CARTESIAN_POINT('Ctrl Pts',(-0.954308486908894,1.67663267125761,0.299111603474267));
#9897=CARTESIAN_POINT('Ctrl Pts',(-0.961833761492987,1.61508042700263,0.273949373987484));
#9898=CARTESIAN_POINT('Ctrl Pts',(-0.963525491562421,1.5815373526696,0.267616567329817));
#9899=CARTESIAN_POINT('Ctrl Pts',(-0.963525491562421,1.5184626473304,0.267616567329817));
#9900=CARTESIAN_POINT('Ctrl Pts',(-0.961833761492987,1.48491957299737,0.273949373987484));
#9901=CARTESIAN_POINT('Ctrl Pts',(-0.954308486908894,1.42336732874239,0.299111603474267));
#9902=CARTESIAN_POINT('Ctrl Pts',(-0.948394987258249,1.39534588636318,0.31788699900678));
#9903=CARTESIAN_POINT('Ctrl Pts',(-0.933155485613026,1.35110381617461,0.360174810895352));
#9904=CARTESIAN_POINT('Ctrl Pts',(-0.92278792026947,1.33188468517318,0.386546956384144));
#9905=CARTESIAN_POINT('Ctrl Pts',(-0.897143218189782,1.30632915724249,0.442820664919227));
#9906=CARTESIAN_POINT('Ctrl Pts',(-0.881791875377343,1.3,0.472691670144998));
#9907=CARTESIAN_POINT('Ctrl Pts',(-0.850258932191534,1.3,0.527308329855002));
#9908=CARTESIAN_POINT('Ctrl Pts',(-0.832065554235658,1.30632915724249,0.555538485325663));
#9909=CARTESIAN_POINT('Ctrl Pts',(-0.796153444118959,1.33188468517318,0.605884303066698));
#9910=CARTESIAN_POINT('Ctrl Pts',(-0.778498278845144,1.35110381617461,0.628048950774009));
#9911=CARTESIAN_POINT('Ctrl Pts',(-0.749495710301795,1.39534588636318,0.662390652284073));
#9912=CARTESIAN_POINT('Ctrl Pts',(-0.73619249062986,1.42336732874239,0.676899590973058));
#9913=CARTESIAN_POINT('Ctrl Pts',(-0.718163997970498,1.48491957299737,0.695997784676727));
#9914=CARTESIAN_POINT('Ctrl Pts',(-0.713525491562421,1.5184626473304,0.700629269222037));
#9915=CARTESIAN_POINT('Ctrl Pts',(-0.713525491562421,1.55,0.700629269222037));
#9916=CARTESIAN_POINT('Origin',(0.,1.55,0.));
#9917=CARTESIAN_POINT('',(0.963525491562421,1.55,-0.267616567329817));
#9918=CARTESIAN_POINT('Ctrl Pts',(0.963525491562421,1.55,-0.267616567329817));
#9919=CARTESIAN_POINT('Ctrl Pts',(0.963525491562421,1.5184626473304,-0.267616567329817));
#9920=CARTESIAN_POINT('Ctrl Pts',(0.961833761492987,1.48491957299737,-0.273949373987484));
#9921=CARTESIAN_POINT('Ctrl Pts',(0.954308486908894,1.42336732874239,-0.299111603474267));
#9922=CARTESIAN_POINT('Ctrl Pts',(0.948394987258249,1.39534588636318,-0.31788699900678));
#9923=CARTESIAN_POINT('Ctrl Pts',(0.933155485613026,1.35110381617461,-0.360174810895352));
#9924=CARTESIAN_POINT('Ctrl Pts',(0.92278792026947,1.33188468517318,-0.386546956384144));
#9925=CARTESIAN_POINT('Ctrl Pts',(0.897143218189782,1.30632915724249,-0.442820664919227));
#9926=CARTESIAN_POINT('Ctrl Pts',(0.881791875377343,1.3,-0.472691670144998));
#9927=CARTESIAN_POINT('Ctrl Pts',(0.850258932191534,1.3,-0.527308329855002));
#9928=CARTESIAN_POINT('Ctrl Pts',(0.832065554235658,1.30632915724249,-0.555538485325663));
#9929=CARTESIAN_POINT('Ctrl Pts',(0.796153444118959,1.33188468517318,-0.605884303066698));
#9930=CARTESIAN_POINT('Ctrl Pts',(0.778498278845144,1.35110381617461,-0.628048950774009));
#9931=CARTESIAN_POINT('Ctrl Pts',(0.749495710301795,1.39534588636318,-0.662390652284073));
#9932=CARTESIAN_POINT('Ctrl Pts',(0.73619249062986,1.42336732874239,-0.676899590973058));
#9933=CARTESIAN_POINT('Ctrl Pts',(0.718163997970498,1.48491957299737,-0.695997784676727));
#9934=CARTESIAN_POINT('Ctrl Pts',(0.713525491562421,1.5184626473304,-0.700629269222037));
#9935=CARTESIAN_POINT('Ctrl Pts',(0.713525491562421,1.5815373526696,-0.700629269222037));
#9936=CARTESIAN_POINT('Ctrl Pts',(0.718163997970498,1.61508042700263,-0.695997784676727));
#9937=CARTESIAN_POINT('Ctrl Pts',(0.73619249062986,1.67663267125761,-0.676899590973058));
#9938=CARTESIAN_POINT('Ctrl Pts',(0.749495710301795,1.70465411363682,-0.662390652284073));
#9939=CARTESIAN_POINT('Ctrl Pts',(0.778498278845144,1.74889618382539,-0.628048950774009));
#9940=CARTESIAN_POINT('Ctrl Pts',(0.796153444118959,1.76811531482682,-0.605884303066698));
#9941=CARTESIAN_POINT('Ctrl Pts',(0.832065554235658,1.79367084275751,-0.555538485325663));
#9942=CARTESIAN_POINT('Ctrl Pts',(0.850258932191534,1.8,-0.527308329855002));
#9943=CARTESIAN_POINT('Ctrl Pts',(0.881791875377343,1.8,-0.472691670144998));
#9944=CARTESIAN_POINT('Ctrl Pts',(0.897143218189782,1.79367084275751,-0.442820664919227));
#9945=CARTESIAN_POINT('Ctrl Pts',(0.92278792026947,1.76811531482682,-0.386546956384144));
#9946=CARTESIAN_POINT('Ctrl Pts',(0.933155485613026,1.74889618382539,-0.360174810895352));
#9947=CARTESIAN_POINT('Ctrl Pts',(0.948394987258249,1.70465411363682,-0.31788699900678));
#9948=CARTESIAN_POINT('Ctrl Pts',(0.954308486908894,1.67663267125761,-0.299111603474267));
#9949=CARTESIAN_POINT('Ctrl Pts',(0.961833761492987,1.61508042700263,-0.273949373987484));
#9950=CARTESIAN_POINT('Ctrl Pts',(0.963525491562421,1.5815373526696,-0.267616567329817));
#9951=CARTESIAN_POINT('Ctrl Pts',(0.963525491562421,1.55,-0.267616567329817));
#9952=CARTESIAN_POINT('',(0.125,1.55,0.21650635094611));
#9953=CARTESIAN_POINT('Origin',(0.,1.55,0.));
#9954=CARTESIAN_POINT('',(-0.25,1.55,-0.968245836551854));
#9955=CARTESIAN_POINT('',(-0.25,1.55,0.));
#9956=CARTESIAN_POINT('Ctrl Pts',(-0.25,1.55,-0.968245836551854));
#9957=CARTESIAN_POINT('Ctrl Pts',(-0.25,1.5815373526696,-0.968245836551854));
#9958=CARTESIAN_POINT('Ctrl Pts',(-0.243669763522489,1.61508042700263,-0.969947158664211));
#9959=CARTESIAN_POINT('Ctrl Pts',(-0.218115996279034,1.67663267125761,-0.976011194447325));
#9960=CARTESIAN_POINT('Ctrl Pts',(-0.198899276956455,1.70465411363682,-0.980277651290853));
#9961=CARTESIAN_POINT('Ctrl Pts',(-0.154657206767882,1.74889618382539,-0.988223761669361));
#9962=CARTESIAN_POINT('Ctrl Pts',(-0.126634476150511,1.76811531482682,-0.992431259450842));
#9963=CARTESIAN_POINT('Ctrl Pts',(-0.0650776639541238,1.79367084275751,
-0.99835915024489));
#9964=CARTESIAN_POINT('Ctrl Pts',(-0.0315329431858092,1.8,-1.));
#9965=CARTESIAN_POINT('Ctrl Pts',(0.0315329431858092,1.8,-1.));
#9966=CARTESIAN_POINT('Ctrl Pts',(0.0650776639541238,1.79367084275751,-0.99835915024489));
#9967=CARTESIAN_POINT('Ctrl Pts',(0.126634476150511,1.76811531482682,-0.992431259450842));
#9968=CARTESIAN_POINT('Ctrl Pts',(0.154657206767882,1.74889618382539,-0.988223761669361));
#9969=CARTESIAN_POINT('Ctrl Pts',(0.198899276956455,1.70465411363682,-0.980277651290853));
#9970=CARTESIAN_POINT('Ctrl Pts',(0.218115996279034,1.67663267125761,-0.976011194447325));
#9971=CARTESIAN_POINT('Ctrl Pts',(0.243669763522488,1.61508042700263,-0.969947158664211));
#9972=CARTESIAN_POINT('Ctrl Pts',(0.25,1.5815373526696,-0.968245836551854));
#9973=CARTESIAN_POINT('Ctrl Pts',(0.25,1.5184626473304,-0.968245836551854));
#9974=CARTESIAN_POINT('Ctrl Pts',(0.243669763522488,1.48491957299737,-0.969947158664211));
#9975=CARTESIAN_POINT('Ctrl Pts',(0.218115996279034,1.42336732874239,-0.976011194447325));
#9976=CARTESIAN_POINT('Ctrl Pts',(0.198899276956455,1.39534588636318,-0.980277651290853));
#9977=CARTESIAN_POINT('Ctrl Pts',(0.154657206767882,1.35110381617461,-0.988223761669361));
#9978=CARTESIAN_POINT('Ctrl Pts',(0.126634476150511,1.33188468517318,-0.992431259450842));
#9979=CARTESIAN_POINT('Ctrl Pts',(0.0650776639541239,1.30632915724249,-0.99835915024489));
#9980=CARTESIAN_POINT('Ctrl Pts',(0.0315329431858092,1.3,-1.));
#9981=CARTESIAN_POINT('Ctrl Pts',(-0.0315329431858092,1.3,-1.));
#9982=CARTESIAN_POINT('Ctrl Pts',(-0.0650776639541239,1.30632915724249,
-0.99835915024489));
#9983=CARTESIAN_POINT('Ctrl Pts',(-0.126634476150511,1.33188468517318,-0.992431259450842));
#9984=CARTESIAN_POINT('Ctrl Pts',(-0.154657206767882,1.35110381617461,-0.988223761669361));
#9985=CARTESIAN_POINT('Ctrl Pts',(-0.198899276956455,1.39534588636318,-0.980277651290853));
#9986=CARTESIAN_POINT('Ctrl Pts',(-0.218115996279034,1.42336732874239,-0.976011194447325));
#9987=CARTESIAN_POINT('Ctrl Pts',(-0.243669763522489,1.48491957299737,-0.969947158664211));
#9988=CARTESIAN_POINT('Ctrl Pts',(-0.25,1.5184626473304,-0.968245836551854));
#9989=CARTESIAN_POINT('Ctrl Pts',(-0.25,1.55,-0.968245836551854));
#9990=CARTESIAN_POINT('Origin',(0.,1.55,0.));
#9991=CARTESIAN_POINT('',(-0.25,1.55,0.968245836551854));
#9992=CARTESIAN_POINT('Ctrl Pts',(-0.25,1.55,0.968245836551854));
#9993=CARTESIAN_POINT('Ctrl Pts',(-0.25,1.5184626473304,0.968245836551854));
#9994=CARTESIAN_POINT('Ctrl Pts',(-0.243669763522489,1.48491957299737,0.969947158664211));
#9995=CARTESIAN_POINT('Ctrl Pts',(-0.218115996279034,1.42336732874239,0.976011194447325));
#9996=CARTESIAN_POINT('Ctrl Pts',(-0.198899276956455,1.39534588636318,0.980277651290853));
#9997=CARTESIAN_POINT('Ctrl Pts',(-0.154657206767882,1.35110381617461,0.988223761669361));
#9998=CARTESIAN_POINT('Ctrl Pts',(-0.126634476150511,1.33188468517318,0.992431259450842));
#9999=CARTESIAN_POINT('Ctrl Pts',(-0.065077663954124,1.30632915724249,0.99835915024489));
#10000=CARTESIAN_POINT('Ctrl Pts',(-0.0315329431858092,1.3,1.));
#10001=CARTESIAN_POINT('Ctrl Pts',(0.0315329431858092,1.3,1.));
#10002=CARTESIAN_POINT('Ctrl Pts',(0.065077663954124,1.30632915724249,0.99835915024489));
#10003=CARTESIAN_POINT('Ctrl Pts',(0.126634476150511,1.33188468517318,0.992431259450842));
#10004=CARTESIAN_POINT('Ctrl Pts',(0.154657206767882,1.35110381617461,0.988223761669361));
#10005=CARTESIAN_POINT('Ctrl Pts',(0.198899276956455,1.39534588636318,0.980277651290853));
#10006=CARTESIAN_POINT('Ctrl Pts',(0.218115996279034,1.42336732874239,0.976011194447325));
#10007=CARTESIAN_POINT('Ctrl Pts',(0.243669763522488,1.48491957299737,0.969947158664211));
#10008=CARTESIAN_POINT('Ctrl Pts',(0.25,1.5184626473304,0.968245836551854));
#10009=CARTESIAN_POINT('Ctrl Pts',(0.25,1.5815373526696,0.968245836551854));
#10010=CARTESIAN_POINT('Ctrl Pts',(0.243669763522488,1.61508042700263,0.969947158664211));
#10011=CARTESIAN_POINT('Ctrl Pts',(0.218115996279034,1.67663267125761,0.976011194447325));
#10012=CARTESIAN_POINT('Ctrl Pts',(0.198899276956455,1.70465411363682,0.980277651290853));
#10013=CARTESIAN_POINT('Ctrl Pts',(0.154657206767882,1.74889618382539,0.988223761669361));
#10014=CARTESIAN_POINT('Ctrl Pts',(0.126634476150511,1.76811531482682,0.992431259450842));
#10015=CARTESIAN_POINT('Ctrl Pts',(0.0650776639541239,1.79367084275751,
0.99835915024489));
#10016=CARTESIAN_POINT('Ctrl Pts',(0.0315329431858092,1.8,1.));
#10017=CARTESIAN_POINT('Ctrl Pts',(-0.0315329431858092,1.8,1.));
#10018=CARTESIAN_POINT('Ctrl Pts',(-0.0650776639541239,1.79367084275751,
0.99835915024489));
#10019=CARTESIAN_POINT('Ctrl Pts',(-0.126634476150511,1.76811531482682,
0.992431259450842));
#10020=CARTESIAN_POINT('Ctrl Pts',(-0.154657206767882,1.74889618382539,
0.988223761669361));
#10021=CARTESIAN_POINT('Ctrl Pts',(-0.198899276956455,1.70465411363682,
0.980277651290853));
#10022=CARTESIAN_POINT('Ctrl Pts',(-0.218115996279034,1.67663267125761,
0.976011194447325));
#10023=CARTESIAN_POINT('Ctrl Pts',(-0.243669763522489,1.61508042700263,
0.969947158664211));
#10024=CARTESIAN_POINT('Ctrl Pts',(-0.25,1.5815373526696,0.968245836551854));
#10025=CARTESIAN_POINT('Ctrl Pts',(-0.25,1.55,0.968245836551854));
#10026=CARTESIAN_POINT('',(-0.25,1.55,0.));
#10027=CARTESIAN_POINT('Origin',(1.65,2.25,0.));
#10028=CARTESIAN_POINT('',(-1.,2.25,-1.22464679914735E-16));
#10029=CARTESIAN_POINT('Origin',(0.,2.25,0.));
#10030=CARTESIAN_POINT('Origin',(1.75,0.85,0.));
#10031=CARTESIAN_POINT('',(-1.75,0.85,-2.14313189850787E-16));
#10032=CARTESIAN_POINT('Origin',(0.,0.85,0.));
#10033=CARTESIAN_POINT('Origin',(0.,0.,0.));
#10034=CARTESIAN_POINT('',(-1.75,-0.85,-2.14313189850787E-16));
#10035=CARTESIAN_POINT('Origin',(0.,-0.85,0.));
#10036=CARTESIAN_POINT('',(-1.75,0.,-2.14313189850787E-16));
#10037=CARTESIAN_POINT('Origin',(1.,-0.85,0.));
#10038=CARTESIAN_POINT('',(-1.,-0.85,-1.22464679914735E-16));
#10039=CARTESIAN_POINT('Origin',(0.,-0.85,0.));
#10040=CARTESIAN_POINT('Origin',(0.,0.7,0.));
#10041=CARTESIAN_POINT('',(-1.,0.7,-1.22464679914735E-16));
#10042=CARTESIAN_POINT('',(0.,0.,0.));
#10043=CARTESIAN_POINT('',(0.,0.,0.));
#10044=CARTESIAN_POINT('',(0.,0.,0.));
#10045=CARTESIAN_POINT('Origin',(0.6,0.8,0.));
#10046=CARTESIAN_POINT('',(-0.6,0.8,-7.34788079488412E-17));
#10047=CARTESIAN_POINT('Origin',(0.,0.8,0.));
#10048=CARTESIAN_POINT('Origin',(0.,0.775,0.));
#10049=CARTESIAN_POINT('',(-0.65,0.75,-7.9602041944578E-17));
#10050=CARTESIAN_POINT('Origin',(0.,0.75,0.));
#10051=CARTESIAN_POINT('',(-0.625,0.775,-7.65404249467096E-17));
#10052=CARTESIAN_POINT('Origin',(0.,0.39,0.));
#10053=CARTESIAN_POINT('',(-0.65,0.0299999999999998,-7.9602041944578E-17));
#10054=CARTESIAN_POINT('Origin',(0.,0.0299999999999998,0.));
#10055=CARTESIAN_POINT('',(-0.65,0.39,-7.9602041944578E-17));
#10056=CARTESIAN_POINT('Origin',(0.,0.0150000000000001,0.));
#10057=CARTESIAN_POINT('',(-0.62,5.89805981832114E-17,-7.59281015471359E-17));
#10058=CARTESIAN_POINT('Origin',(0.,0.,0.));
#10059=CARTESIAN_POINT('',(-0.635,0.0150000000000001,-7.77650717458569E-17));
#10060=CARTESIAN_POINT('Origin',(0.42,0.,0.));
#10061=CARTESIAN_POINT('',(-0.42,-3.46944695195361E-18,-5.14351655641888E-17));
#10062=CARTESIAN_POINT('Origin',(0.,0.,0.));
#10063=CARTESIAN_POINT('Origin',(0.,-0.02,0.));
#10064=CARTESIAN_POINT('',(-0.3933,-0.0534000000000001,4.81653586104654E-17));
#10065=CARTESIAN_POINT('Origin',(0.,-0.0534000000000001,0.));
#10066=CARTESIAN_POINT('',(-0.41,-0.02,-5.02105187650415E-17));
#10067=CARTESIAN_POINT('Origin',(0.,-1.48,0.));
#10068=CARTESIAN_POINT('',(-0.3933,-2.9267,4.81653586104654E-17));
#10069=CARTESIAN_POINT('Origin',(0.,-2.9267,0.));
#10070=CARTESIAN_POINT('',(-0.3933,-1.48,-4.81653586104654E-17));
#10071=CARTESIAN_POINT('Origin',(0.,-2.96,0.));
#10072=CARTESIAN_POINT('',(-0.32,-3.,-3.91886975727153E-17));
#10073=CARTESIAN_POINT('Origin',(0.,-3.,0.));
#10074=CARTESIAN_POINT('',(-0.36,-2.96,-4.40872847693047E-17));
#10075=CARTESIAN_POINT('Origin',(0.,-3.,0.));
#10076=CARTESIAN_POINT('Origin',(0.173205080756888,-0.8,-0.3));
#10077=CARTESIAN_POINT('',(0.346410161513775,-0.8,0.));
#10078=CARTESIAN_POINT('',(0.173205080756888,-0.8,-0.3));
#10079=CARTESIAN_POINT('',(0.346410161513775,-0.8,0.));
#10080=CARTESIAN_POINT('',(0.173205080756888,-1.28,-0.3));
#10081=CARTESIAN_POINT('',(0.173205080756888,-0.8,-0.3));
#10082=CARTESIAN_POINT('',(0.346410161513775,-1.28,0.));
#10083=CARTESIAN_POINT('',(0.346410161513775,-1.28,0.));
#10084=CARTESIAN_POINT('',(0.346410161513775,-0.8,0.));
#10085=CARTESIAN_POINT('Origin',(-0.173205080756888,-0.8,-0.3));
#10086=CARTESIAN_POINT('',(-0.173205080756888,-0.8,-0.3));
#10087=CARTESIAN_POINT('',(0.173205080756888,-0.8,-0.3));
#10088=CARTESIAN_POINT('',(-0.173205080756888,-1.28,-0.3));
#10089=CARTESIAN_POINT('',(-0.173205080756888,-0.8,-0.3));
#10090=CARTESIAN_POINT('',(0.173205080756888,-1.28,-0.3));
#10091=CARTESIAN_POINT('Origin',(-0.346410161513775,-0.8,-5.55111512312578E-17));
#10092=CARTESIAN_POINT('',(-0.346410161513775,-0.8,-4.24230095489963E-17));
#10093=CARTESIAN_POINT('',(-0.173205080756888,-0.8,-0.3));
#10094=CARTESIAN_POINT('',(-0.346410161513775,-1.28,-5.55111512312578E-17));
#10095=CARTESIAN_POINT('',(-0.346410161513775,-0.8,-4.24230095489963E-17));
#10096=CARTESIAN_POINT('',(-0.173205080756888,-1.28,-0.3));
#10097=CARTESIAN_POINT('Origin',(-0.173205080756888,-0.8,0.3));
#10098=CARTESIAN_POINT('',(-0.173205080756888,-0.8,0.3));
#10099=CARTESIAN_POINT('',(-0.346410161513775,-0.8,-4.24230095489963E-17));
#10100=CARTESIAN_POINT('',(-0.173205080756888,-1.28,0.3));
#10101=CARTESIAN_POINT('',(-0.173205080756888,-0.8,0.3));
#10102=CARTESIAN_POINT('',(-0.346410161513775,-1.28,-4.24230095489963E-17));
#10103=CARTESIAN_POINT('Origin',(0.173205080756888,-0.8,0.3));
#10104=CARTESIAN_POINT('',(0.173205080756888,-0.8,0.3));
#10105=CARTESIAN_POINT('',(-0.173205080756888,-0.8,0.3));
#10106=CARTESIAN_POINT('',(0.173205080756888,-1.28,0.3));
#10107=CARTESIAN_POINT('',(0.173205080756888,-0.8,0.3));
#10108=CARTESIAN_POINT('',(-0.173205080756888,-1.28,0.3));
#10109=CARTESIAN_POINT('Origin',(0.346410161513775,-0.8,0.));
#10110=CARTESIAN_POINT('',(0.173205080756888,-0.8,0.3));
#10111=CARTESIAN_POINT('',(0.173205080756888,-1.28,0.3));
#10112=CARTESIAN_POINT('Origin',(0.,-0.8,-5.55111512312578E-17));
#10113=CARTESIAN_POINT('Origin',(0.,-1.28,-5.55111512312578E-17));
#10114=CARTESIAN_POINT('',(0.,0.,0.));
#10115=CARTESIAN_POINT('',(0.,0.,0.));
#10116=CARTESIAN_POINT('Origin',(-0.3,4.,6.9));
#10117=CARTESIAN_POINT('',(-0.3,6.,7.04606079858305));
#10118=CARTESIAN_POINT('',(-0.3,4.,7.04606079858305));
#10119=CARTESIAN_POINT('',(-0.3,-4.5,7.04606079858305));
#10120=CARTESIAN_POINT('',(-0.3,6.,7.35));
#10121=CARTESIAN_POINT('',(-0.3,6.,7.35));
#10122=CARTESIAN_POINT('',(-0.3,4.,7.35));
#10123=CARTESIAN_POINT('',(-0.3,4.,7.35));
#10124=CARTESIAN_POINT('',(-0.3,4.,7.35));
#10125=CARTESIAN_POINT('Origin',(0.,4.,7.125));
#10126=CARTESIAN_POINT('',(0.3,4.,7.04606079858305));
#10127=CARTESIAN_POINT('Origin',(0.,4.,8.));
#10128=CARTESIAN_POINT('',(0.3,4.,7.35));
#10129=CARTESIAN_POINT('',(0.3,4.,7.35));
#10130=CARTESIAN_POINT('',(0.3,4.,6.9));
#10131=CARTESIAN_POINT('Origin',(0.3,4.,7.35));
#10132=CARTESIAN_POINT('',(0.3,6.,7.04606079858305));
#10133=CARTESIAN_POINT('',(0.3,-4.5,7.04606079858305));
#10134=CARTESIAN_POINT('',(0.3,6.,7.35));
#10135=CARTESIAN_POINT('',(0.3,4.,7.35));
#10136=CARTESIAN_POINT('',(0.3,6.,6.9));
#10137=CARTESIAN_POINT('Origin',(-0.3,4.,7.35));
#10138=CARTESIAN_POINT('',(0.3,6.,7.35));
#10139=CARTESIAN_POINT('Origin',(0.,6.,7.125));
#10140=CARTESIAN_POINT('Origin',(0.,6.,8.));
#10141=CARTESIAN_POINT('Origin',(0.,-7.1,8.));
#10142=CARTESIAN_POINT('',(-0.21,-7.,8.));
#10143=CARTESIAN_POINT('Origin',(0.,-7.,8.));
#10144=CARTESIAN_POINT('',(-0.21,-5.,8.));
#10145=CARTESIAN_POINT('',(-0.21,-7.1,8.));
#10146=CARTESIAN_POINT('Origin',(0.,-5.,8.));
#10147=CARTESIAN_POINT('Origin',(0.,-5.,8.));
#10148=CARTESIAN_POINT('Origin',(-0.2,-6.55,7.3));
#10149=CARTESIAN_POINT('',(-0.2,-5.1,7.43431457505076));
#10150=CARTESIAN_POINT('',(-0.2,-6.55,7.43431457505076));
#10151=CARTESIAN_POINT('',(-0.2,-7.,7.43431457505076));
#10152=CARTESIAN_POINT('',(-0.2,-5.1,7.65));
#10153=CARTESIAN_POINT('',(-0.2,-5.1,7.65));
#10154=CARTESIAN_POINT('',(-0.2,-6.55,7.65));
#10155=CARTESIAN_POINT('',(-0.2,-6.55,7.65));
#10156=CARTESIAN_POINT('',(-0.2,-6.55,7.65));
#10157=CARTESIAN_POINT('Origin',(0.,-6.55,7.475));
#10158=CARTESIAN_POINT('',(0.2,-6.55,7.43431457505076));
#10159=CARTESIAN_POINT('Origin',(0.,-6.55,8.));
#10160=CARTESIAN_POINT('',(0.2,-6.55,7.65));
#10161=CARTESIAN_POINT('',(0.2,-6.55,7.65));
#10162=CARTESIAN_POINT('',(0.2,-6.55,7.3));
#10163=CARTESIAN_POINT('Origin',(0.2,-6.55,7.65));
#10164=CARTESIAN_POINT('',(0.2,-5.1,7.43431457505076));
#10165=CARTESIAN_POINT('',(0.2,-7.,7.43431457505076));
#10166=CARTESIAN_POINT('',(0.2,-5.1,7.65));
#10167=CARTESIAN_POINT('',(0.2,-6.55,7.65));
#10168=CARTESIAN_POINT('',(0.2,-5.1,7.3));
#10169=CARTESIAN_POINT('Origin',(-0.2,-6.55,7.65));
#10170=CARTESIAN_POINT('',(0.2,-5.1,7.65));
#10171=CARTESIAN_POINT('Origin',(0.,-5.1,7.475));
#10172=CARTESIAN_POINT('Origin',(0.,-5.1,8.));
#10173=CARTESIAN_POINT('Origin',(0.,6.5,8.));
#10174=CARTESIAN_POINT('',(-0.4,7.8,8.));
#10175=CARTESIAN_POINT('Origin',(0.,7.8,8.));
#10176=CARTESIAN_POINT('',(-0.4,6.5,8.));
#10177=CARTESIAN_POINT('',(-0.4,6.5,8.));
#10178=CARTESIAN_POINT('Origin',(0.,6.5,8.));
#10179=CARTESIAN_POINT('Origin',(0.,7.8,8.));
#10180=CARTESIAN_POINT('Origin',(0.,-7.,8.));
#10181=CARTESIAN_POINT('',(-0.6,-4.5,8.));
#10182=CARTESIAN_POINT('Origin',(0.,-4.5,8.));
#10183=CARTESIAN_POINT('',(-0.6,-7.,8.));
#10184=CARTESIAN_POINT('',(-0.6,-7.,8.));
#10185=CARTESIAN_POINT('Origin',(0.,-7.,8.));
#10186=CARTESIAN_POINT('Origin',(0.,-7.,8.));
#10187=CARTESIAN_POINT('Origin',(0.,-4.5,8.));
#10188=CARTESIAN_POINT('',(-1.,6.5,8.));
#10189=CARTESIAN_POINT('Origin',(0.,6.5,8.));
#10190=CARTESIAN_POINT('',(-1.,-4.5,8.));
#10191=CARTESIAN_POINT('',(-1.,-4.5,8.));
#10192=CARTESIAN_POINT('Origin',(0.,-4.5,8.));
#10193=CARTESIAN_POINT('Origin',(0.,6.5,8.));
#10194=CARTESIAN_POINT('Origin',(0.,-4.5,8.));
#10195=CARTESIAN_POINT('',(0.,0.,0.));
#10196=CARTESIAN_POINT('Origin',(0.,-4.95,8.));
#10197=CARTESIAN_POINT('',(-0.605,-4.5,8.));
#10198=CARTESIAN_POINT('Origin',(0.,-4.5,8.));
#10199=CARTESIAN_POINT('',(-0.605,-4.95,8.));
#10200=CARTESIAN_POINT('',(-0.605,-4.95,8.));
#10201=CARTESIAN_POINT('Origin',(0.,-4.95,8.));
#10202=CARTESIAN_POINT('Origin',(0.,-4.95,8.));
#10203=CARTESIAN_POINT('',(-0.9,-4.5,8.));
#10204=CARTESIAN_POINT('Origin',(0.,-4.5,8.));
#10205=CARTESIAN_POINT('',(-0.9,-4.95,8.));
#10206=CARTESIAN_POINT('',(-0.9,-4.95,8.));
#10207=CARTESIAN_POINT('Origin',(0.,-4.95,8.));
#10208=CARTESIAN_POINT('Origin',(0.,-4.5,8.));
#10209=CARTESIAN_POINT('Origin',(0.,-4.95,8.));
#10210=CARTESIAN_POINT('',(0.,0.,0.));
#10211=CARTESIAN_POINT('Origin',(0.,-7.,8.));
#10212=CARTESIAN_POINT('',(-0.605,-6.7,8.));
#10213=CARTESIAN_POINT('Origin',(0.,-6.7,8.));
#10214=CARTESIAN_POINT('',(-0.605,-7.,8.));
#10215=CARTESIAN_POINT('',(-0.605,-7.,8.));
#10216=CARTESIAN_POINT('Origin',(0.,-7.,8.));
#10217=CARTESIAN_POINT('Origin',(0.,-7.,8.));
#10218=CARTESIAN_POINT('',(-0.9,-6.7,8.));
#10219=CARTESIAN_POINT('Origin',(0.,-6.7,8.));
#10220=CARTESIAN_POINT('',(-0.9,-7.,8.));
#10221=CARTESIAN_POINT('',(-0.9,-7.,8.));
#10222=CARTESIAN_POINT('Origin',(0.,-7.,8.));
#10223=CARTESIAN_POINT('Origin',(0.,-6.7,8.));
#10224=CARTESIAN_POINT('Origin',(0.,-7.,8.));
#10225=CARTESIAN_POINT('',(0.,0.,0.));
#10226=CARTESIAN_POINT('Origin',(0.,-7.2,8.));
#10227=CARTESIAN_POINT('',(-0.275,-7.,8.));
#10228=CARTESIAN_POINT('Origin',(0.,-7.,8.));
#10229=CARTESIAN_POINT('',(-0.275,-7.2,8.));
#10230=CARTESIAN_POINT('',(-0.275,-7.2,8.));
#10231=CARTESIAN_POINT('Origin',(0.,-7.2,8.));
#10232=CARTESIAN_POINT('Origin',(0.,-7.2,8.));
#10233=CARTESIAN_POINT('',(-1.,-7.,8.));
#10234=CARTESIAN_POINT('Origin',(0.,-7.,8.));
#10235=CARTESIAN_POINT('',(-1.,-7.2,8.));
#10236=CARTESIAN_POINT('',(-1.,-7.2,8.));
#10237=CARTESIAN_POINT('Origin',(0.,-7.2,8.));
#10238=CARTESIAN_POINT('Origin',(0.,-7.,8.));
#10239=CARTESIAN_POINT('Origin',(0.,-7.2,8.));
#10240=CARTESIAN_POINT('',(0.,0.,0.));
#10241=CARTESIAN_POINT('Origin',(0.,-1.25,8.99));
#10242=CARTESIAN_POINT('',(0.172988438920061,-1.36905880899791,8.99));
#10243=CARTESIAN_POINT('',(0.172988438920061,-1.13094119100209,8.99));
#10244=CARTESIAN_POINT('',(0.172988438920061,-1.65,8.99));
#10245=CARTESIAN_POINT('Origin',(0.,-1.25,8.99));
#10246=CARTESIAN_POINT('Origin',(0.,-1.25,8.99));
#10247=CARTESIAN_POINT('',(-0.172988438920061,-1.36905880899791,8.99));
#10248=CARTESIAN_POINT('Ctrl Pts',(-0.172988438920061,-1.36905880899791,
8.99));
#10249=CARTESIAN_POINT('Ctrl Pts',(-0.165594865311318,-1.37980142239529,
8.99129192197638));
#10250=CARTESIAN_POINT('Ctrl Pts',(-0.157297138725608,-1.38968770937274,
8.99265394943905));
#10251=CARTESIAN_POINT('Ctrl Pts',(-0.129892073845076,-1.41709277425327,
8.9967480843909));
#10252=CARTESIAN_POINT('Ctrl Pts',(-0.106330167759284,-1.43324205633295,
8.99969589327638));
#10253=CARTESIAN_POINT('Ctrl Pts',(-0.0546129046324105,-1.45469779396491,
9.00385029472357));
#10254=CARTESIAN_POINT('Ctrl Pts',(-0.0264512308298517,-1.46,9.005));
#10255=CARTESIAN_POINT('Ctrl Pts',(0.0264512308298516,-1.46,9.005));
#10256=CARTESIAN_POINT('Ctrl Pts',(0.0546129046324105,-1.45469779396491,
9.00385029472357));
#10257=CARTESIAN_POINT('Ctrl Pts',(0.106330167759284,-1.43324205633295,
8.99969589327638));
#10258=CARTESIAN_POINT('Ctrl Pts',(0.129892073845076,-1.41709277425327,
8.9967480843909));
#10259=CARTESIAN_POINT('Ctrl Pts',(0.157297138725608,-1.38968770937274,
8.99265394943905));
#10260=CARTESIAN_POINT('Ctrl Pts',(0.165594865311318,-1.37980142239529,
8.99129192197638));
#10261=CARTESIAN_POINT('Ctrl Pts',(0.172988438920061,-1.36905880899791,
8.99));
#10262=CARTESIAN_POINT('',(-0.21,-1.25,8.99));
#10263=CARTESIAN_POINT('Origin',(0.,-1.25,8.99));
#10264=CARTESIAN_POINT('',(-0.21,-1.25,9.48522725533839));
#10265=CARTESIAN_POINT('',(-0.21,-1.25,8.99));
#10266=CARTESIAN_POINT('',(0.21,-1.25,9.48522725533839));
#10267=CARTESIAN_POINT('Ctrl Pts',(0.21,-1.25,9.48522725533839));
#10268=CARTESIAN_POINT('Ctrl Pts',(0.21,-1.27640552692445,9.48522725533839));
#10269=CARTESIAN_POINT('Ctrl Pts',(0.204715737269596,-1.30454707409071,
9.48600415954412));
#10270=CARTESIAN_POINT('Ctrl Pts',(0.183273763036331,-1.35627626890513,
9.48880073282317));
#10271=CARTESIAN_POINT('Ctrl Pts',(0.167117923970394,-1.37986692412796,
9.49077897157582));
#10272=CARTESIAN_POINT('Ctrl Pts',(0.129867169887369,-1.41711767821098,
9.49448481141327));
#10273=CARTESIAN_POINT('Ctrl Pts',(0.106276408305765,-1.43327371000135,
9.49645455657129));
#10274=CARTESIAN_POINT('Ctrl Pts',(0.0545468514059002,-1.45471582482622,
9.49923165515646));
#10275=CARTESIAN_POINT('Ctrl Pts',(0.0264051785092814,-1.46,9.5));
#10276=CARTESIAN_POINT('Ctrl Pts',(-0.0264051785092814,-1.46,9.5));
#10277=CARTESIAN_POINT('Ctrl Pts',(-0.0545468514059001,-1.45471582482622,
9.49923165515646));
#10278=CARTESIAN_POINT('Ctrl Pts',(-0.106276408305765,-1.43327371000135,
9.49645455657129));
#10279=CARTESIAN_POINT('Ctrl Pts',(-0.129867169887369,-1.41711767821098,
9.49448481141327));
#10280=CARTESIAN_POINT('Ctrl Pts',(-0.167117923970394,-1.37986692412796,
9.49077897157582));
#10281=CARTESIAN_POINT('Ctrl Pts',(-0.183273763036331,-1.35627626890513,
9.48880073282317));
#10282=CARTESIAN_POINT('Ctrl Pts',(-0.204715737269596,-1.30454707409071,
9.48600415954412));
#10283=CARTESIAN_POINT('Ctrl Pts',(-0.21,-1.27640552692445,9.48522725533839));
#10284=CARTESIAN_POINT('Ctrl Pts',(-0.21,-1.25,9.48522725533839));
#10285=CARTESIAN_POINT('Ctrl Pts',(-0.21,-1.25,9.48522725533839));
#10286=CARTESIAN_POINT('Ctrl Pts',(-0.21,-1.22359447307555,9.48522725533839));
#10287=CARTESIAN_POINT('Ctrl Pts',(-0.204715737269596,-1.19545292590929,
9.48600415954412));
#10288=CARTESIAN_POINT('Ctrl Pts',(-0.183273763036331,-1.14372373109487,
9.48880073282317));
#10289=CARTESIAN_POINT('Ctrl Pts',(-0.167117923970394,-1.12013307587204,
9.49077897157582));
#10290=CARTESIAN_POINT('Ctrl Pts',(-0.129867169887369,-1.08288232178902,
9.49448481141327));
#10291=CARTESIAN_POINT('Ctrl Pts',(-0.106276408305765,-1.06672628999865,
9.49645455657129));
#10292=CARTESIAN_POINT('Ctrl Pts',(-0.0545468514059002,-1.04528417517378,
9.49923165515646));
#10293=CARTESIAN_POINT('Ctrl Pts',(-0.0264051785092814,-1.04,9.5));
#10294=CARTESIAN_POINT('Ctrl Pts',(0.0264051785092814,-1.04,9.5));
#10295=CARTESIAN_POINT('Ctrl Pts',(0.0545468514059002,-1.04528417517378,
9.49923165515645));
#10296=CARTESIAN_POINT('Ctrl Pts',(0.106276408305765,-1.06672628999865,
9.49645455657129));
#10297=CARTESIAN_POINT('Ctrl Pts',(0.129867169887369,-1.08288232178902,
9.49448481141327));
#10298=CARTESIAN_POINT('Ctrl Pts',(0.167117923970394,-1.12013307587204,
9.49077897157582));
#10299=CARTESIAN_POINT('Ctrl Pts',(0.183273763036332,-1.14372373109487,
9.48880073282317));
#10300=CARTESIAN_POINT('Ctrl Pts',(0.204715737269596,-1.19545292590929,
9.48600415954412));
#10301=CARTESIAN_POINT('Ctrl Pts',(0.21,-1.22359447307555,9.48522725533839));
#10302=CARTESIAN_POINT('Ctrl Pts',(0.21,-1.25,9.48522725533839));
#10303=CARTESIAN_POINT('',(-0.172988438920061,-1.13094119100209,8.99));
#10304=CARTESIAN_POINT('Origin',(0.,-1.25,8.99));
#10305=CARTESIAN_POINT('Ctrl Pts',(0.172988438920061,-1.13094119100209,
8.99));
#10306=CARTESIAN_POINT('Ctrl Pts',(0.165594865311318,-1.12019857760471,
8.99129192197638));
#10307=CARTESIAN_POINT('Ctrl Pts',(0.157297138725608,-1.11031229062726,
8.99265394943905));
#10308=CARTESIAN_POINT('Ctrl Pts',(0.129892073845076,-1.08290722574673,
8.9967480843909));
#10309=CARTESIAN_POINT('Ctrl Pts',(0.106330167759284,-1.06675794366705,
8.99969589327638));
#10310=CARTESIAN_POINT('Ctrl Pts',(0.0546129046324105,-1.04530220603509,
9.00385029472357));
#10311=CARTESIAN_POINT('Ctrl Pts',(0.0264512308298516,-1.04,9.005));
#10312=CARTESIAN_POINT('Ctrl Pts',(-0.0264512308298516,-1.04,9.005));
#10313=CARTESIAN_POINT('Ctrl Pts',(-0.0546129046324105,-1.04530220603509,
9.00385029472357));
#10314=CARTESIAN_POINT('Ctrl Pts',(-0.106330167759284,-1.06675794366705,
8.99969589327638));
#10315=CARTESIAN_POINT('Ctrl Pts',(-0.129892073845076,-1.08290722574673,
8.9967480843909));
#10316=CARTESIAN_POINT('Ctrl Pts',(-0.157297138725608,-1.11031229062726,
8.99265394943905));
#10317=CARTESIAN_POINT('Ctrl Pts',(-0.165594865311318,-1.12019857760471,
8.99129192197638));
#10318=CARTESIAN_POINT('Ctrl Pts',(-0.172988438920061,-1.13094119100209,
8.99));
#10319=CARTESIAN_POINT('Origin',(0.,-1.25,8.99));
#10320=CARTESIAN_POINT('',(-0.172988438920061,-1.65,8.99));
#10321=CARTESIAN_POINT('Origin',(0.,-1.65,8.));
#10322=CARTESIAN_POINT('',(-1.005,-0.85,8.));
#10323=CARTESIAN_POINT('Origin',(0.,-0.85,8.));
#10324=CARTESIAN_POINT('',(-1.005,-1.65,8.));
#10325=CARTESIAN_POINT('',(-1.005,-1.65,8.));
#10326=CARTESIAN_POINT('Origin',(0.,-1.65,8.));
#10327=CARTESIAN_POINT('Origin',(0.,-1.65,8.));
#10328=CARTESIAN_POINT('',(-1.5,-0.85,8.));
#10329=CARTESIAN_POINT('Origin',(0.,-0.85,8.));
#10330=CARTESIAN_POINT('',(-1.5,-1.65,8.));
#10331=CARTESIAN_POINT('',(-1.5,-1.65,8.));
#10332=CARTESIAN_POINT('Origin',(0.,-1.65,8.));
#10333=CARTESIAN_POINT('Origin',(0.,-0.85,8.));
#10334=CARTESIAN_POINT('Origin',(0.,-1.65,8.));
#10335=CARTESIAN_POINT('',(0.,0.,0.));
#10336=CARTESIAN_POINT('Origin',(0.,2.85,8.99));
#10337=CARTESIAN_POINT('',(0.172988438920061,2.73094119100209,8.99));
#10338=CARTESIAN_POINT('',(0.172988438920061,2.96905880899791,8.99));
#10339=CARTESIAN_POINT('',(0.172988438920061,2.45,8.99));
#10340=CARTESIAN_POINT('Origin',(0.,2.85,8.99));
#10341=CARTESIAN_POINT('Origin',(0.,2.85,8.99));
#10342=CARTESIAN_POINT('',(-0.172988438920061,2.73094119100209,8.99));
#10343=CARTESIAN_POINT('Ctrl Pts',(-0.172988438920061,2.73094119100209,
8.99));
#10344=CARTESIAN_POINT('Ctrl Pts',(-0.165594865311318,2.72019857760471,
8.99129192197638));
#10345=CARTESIAN_POINT('Ctrl Pts',(-0.157297138725608,2.71031229062726,
8.99265394943905));
#10346=CARTESIAN_POINT('Ctrl Pts',(-0.129892073845076,2.68290722574673,
8.9967480843909));
#10347=CARTESIAN_POINT('Ctrl Pts',(-0.106330167759285,2.66675794366705,
8.99969589327638));
#10348=CARTESIAN_POINT('Ctrl Pts',(-0.0546129046324105,2.64530220603509,
9.00385029472357));
#10349=CARTESIAN_POINT('Ctrl Pts',(-0.0264512308298517,2.64,9.005));
#10350=CARTESIAN_POINT('Ctrl Pts',(0.0264512308298516,2.64,9.005));
#10351=CARTESIAN_POINT('Ctrl Pts',(0.0546129046324104,2.64530220603509,
9.00385029472357));
#10352=CARTESIAN_POINT('Ctrl Pts',(0.106330167759284,2.66675794366705,8.99969589327638));
#10353=CARTESIAN_POINT('Ctrl Pts',(0.129892073845076,2.68290722574673,8.9967480843909));
#10354=CARTESIAN_POINT('Ctrl Pts',(0.157297138725608,2.71031229062726,8.99265394943905));
#10355=CARTESIAN_POINT('Ctrl Pts',(0.165594865311318,2.72019857760471,8.99129192197638));
#10356=CARTESIAN_POINT('Ctrl Pts',(0.172988438920061,2.73094119100209,8.99));
#10357=CARTESIAN_POINT('',(-0.21,2.85,8.99));
#10358=CARTESIAN_POINT('Origin',(0.,2.85,8.99));
#10359=CARTESIAN_POINT('',(-0.21,2.85,9.48522725533839));
#10360=CARTESIAN_POINT('',(-0.21,2.85,8.99));
#10361=CARTESIAN_POINT('',(0.21,2.85,9.48522725533839));
#10362=CARTESIAN_POINT('Ctrl Pts',(0.21,2.85,9.48522725533839));
#10363=CARTESIAN_POINT('Ctrl Pts',(0.21,2.82359447307555,9.48522725533839));
#10364=CARTESIAN_POINT('Ctrl Pts',(0.204715737269596,2.79545292590929,9.48600415954412));
#10365=CARTESIAN_POINT('Ctrl Pts',(0.183273763036332,2.74372373109487,9.48880073282317));
#10366=CARTESIAN_POINT('Ctrl Pts',(0.167117923970394,2.72013307587204,9.49077897157582));
#10367=CARTESIAN_POINT('Ctrl Pts',(0.129867169887369,2.68288232178902,9.49448481141327));
#10368=CARTESIAN_POINT('Ctrl Pts',(0.106276408305765,2.66672628999865,9.49645455657129));
#10369=CARTESIAN_POINT('Ctrl Pts',(0.0545468514059001,2.64528417517378,
9.49923165515646));
#10370=CARTESIAN_POINT('Ctrl Pts',(0.0264051785092814,2.64,9.5));
#10371=CARTESIAN_POINT('Ctrl Pts',(-0.0264051785092814,2.64,9.5));
#10372=CARTESIAN_POINT('Ctrl Pts',(-0.0545468514059001,2.64528417517378,
9.49923165515646));
#10373=CARTESIAN_POINT('Ctrl Pts',(-0.106276408305765,2.66672628999865,
9.49645455657129));
#10374=CARTESIAN_POINT('Ctrl Pts',(-0.129867169887369,2.68288232178902,
9.49448481141327));
#10375=CARTESIAN_POINT('Ctrl Pts',(-0.167117923970394,2.72013307587204,
9.49077897157582));
#10376=CARTESIAN_POINT('Ctrl Pts',(-0.183273763036332,2.74372373109487,
9.48880073282317));
#10377=CARTESIAN_POINT('Ctrl Pts',(-0.204715737269596,2.79545292590929,
9.48600415954412));
#10378=CARTESIAN_POINT('Ctrl Pts',(-0.21,2.82359447307555,9.48522725533839));
#10379=CARTESIAN_POINT('Ctrl Pts',(-0.21,2.85,9.48522725533839));
#10380=CARTESIAN_POINT('Ctrl Pts',(-0.21,2.85,9.48522725533839));
#10381=CARTESIAN_POINT('Ctrl Pts',(-0.21,2.87640552692445,9.48522725533839));
#10382=CARTESIAN_POINT('Ctrl Pts',(-0.204715737269596,2.90454707409071,
9.48600415954412));
#10383=CARTESIAN_POINT('Ctrl Pts',(-0.183273763036332,2.95627626890513,
9.48880073282317));
#10384=CARTESIAN_POINT('Ctrl Pts',(-0.167117923970394,2.97986692412796,
9.49077897157582));
#10385=CARTESIAN_POINT('Ctrl Pts',(-0.129867169887369,3.01711767821098,
9.49448481141327));
#10386=CARTESIAN_POINT('Ctrl Pts',(-0.106276408305765,3.03327371000135,
9.49645455657129));
#10387=CARTESIAN_POINT('Ctrl Pts',(-0.0545468514059001,3.05471582482622,
9.49923165515646));
#10388=CARTESIAN_POINT('Ctrl Pts',(-0.0264051785092814,3.06,9.5));
#10389=CARTESIAN_POINT('Ctrl Pts',(0.0264051785092814,3.06,9.5));
#10390=CARTESIAN_POINT('Ctrl Pts',(0.0545468514059005,3.05471582482622,
9.49923165515645));
#10391=CARTESIAN_POINT('Ctrl Pts',(0.106276408305765,3.03327371000135,9.49645455657129));
#10392=CARTESIAN_POINT('Ctrl Pts',(0.129867169887369,3.01711767821098,9.49448481141327));
#10393=CARTESIAN_POINT('Ctrl Pts',(0.167117923970394,2.97986692412796,9.49077897157582));
#10394=CARTESIAN_POINT('Ctrl Pts',(0.183273763036332,2.95627626890513,9.48880073282317));
#10395=CARTESIAN_POINT('Ctrl Pts',(0.204715737269596,2.90454707409071,9.48600415954412));
#10396=CARTESIAN_POINT('Ctrl Pts',(0.21,2.87640552692445,9.48522725533839));
#10397=CARTESIAN_POINT('Ctrl Pts',(0.21,2.85,9.48522725533839));
#10398=CARTESIAN_POINT('',(-0.172988438920061,2.96905880899791,8.99));
#10399=CARTESIAN_POINT('Origin',(0.,2.85,8.99));
#10400=CARTESIAN_POINT('Ctrl Pts',(0.172988438920061,2.96905880899791,8.99));
#10401=CARTESIAN_POINT('Ctrl Pts',(0.165594865311318,2.97980142239529,8.99129192197638));
#10402=CARTESIAN_POINT('Ctrl Pts',(0.157297138725609,2.98968770937274,8.99265394943905));
#10403=CARTESIAN_POINT('Ctrl Pts',(0.129892073845076,3.01709277425327,8.9967480843909));
#10404=CARTESIAN_POINT('Ctrl Pts',(0.106330167759284,3.03324205633295,8.99969589327638));
#10405=CARTESIAN_POINT('Ctrl Pts',(0.0546129046324105,3.05469779396491,
9.00385029472357));
#10406=CARTESIAN_POINT('Ctrl Pts',(0.0264512308298516,3.06,9.005));
#10407=CARTESIAN_POINT('Ctrl Pts',(-0.0264512308298516,3.06,9.005));
#10408=CARTESIAN_POINT('Ctrl Pts',(-0.0546129046324104,3.05469779396491,
9.00385029472357));
#10409=CARTESIAN_POINT('Ctrl Pts',(-0.106330167759284,3.03324205633295,
8.99969589327638));
#10410=CARTESIAN_POINT('Ctrl Pts',(-0.129892073845076,3.01709277425327,
8.9967480843909));
#10411=CARTESIAN_POINT('Ctrl Pts',(-0.157297138725609,2.98968770937274,
8.99265394943905));
#10412=CARTESIAN_POINT('Ctrl Pts',(-0.165594865311319,2.97980142239529,
8.99129192197638));
#10413=CARTESIAN_POINT('Ctrl Pts',(-0.172988438920062,2.96905880899791,
8.99));
#10414=CARTESIAN_POINT('Origin',(0.,2.85,8.99));
#10415=CARTESIAN_POINT('',(-0.172988438920061,2.45,8.99));
#10416=CARTESIAN_POINT('Origin',(0.,2.45,8.));
#10417=CARTESIAN_POINT('',(-1.005,3.25,8.));
#10418=CARTESIAN_POINT('Origin',(0.,3.25,8.));
#10419=CARTESIAN_POINT('',(-1.005,2.45,8.));
#10420=CARTESIAN_POINT('',(-1.005,2.45,8.));
#10421=CARTESIAN_POINT('Origin',(0.,2.45,8.));
#10422=CARTESIAN_POINT('Origin',(0.,2.45,8.));
#10423=CARTESIAN_POINT('',(-1.5,3.25,8.));
#10424=CARTESIAN_POINT('Origin',(0.,3.25,8.));
#10425=CARTESIAN_POINT('',(-1.5,2.45,8.));
#10426=CARTESIAN_POINT('',(-1.5,2.45,8.));
#10427=CARTESIAN_POINT('Origin',(0.,2.45,8.));
#10428=CARTESIAN_POINT('Origin',(0.,3.25,8.));
#10429=CARTESIAN_POINT('Origin',(0.,2.45,8.));
#10430=CARTESIAN_POINT('',(0.,0.,0.));
#10431=CARTESIAN_POINT('Origin',(-0.3,3.4,6.72));
#10432=CARTESIAN_POINT('',(-0.3,3.5,6.72));
#10433=CARTESIAN_POINT('',(-0.3,3.5,7.04606079858305));
#10434=CARTESIAN_POINT('',(-0.3,3.5,7.36));
#10435=CARTESIAN_POINT('',(-0.3,6.5,6.72));
#10436=CARTESIAN_POINT('',(-0.3,3.4,6.72));
#10437=CARTESIAN_POINT('',(-0.3,6.5,7.04606079858305));
#10438=CARTESIAN_POINT('',(-0.3,6.5,7.36));
#10439=CARTESIAN_POINT('',(-0.3,3.5,7.04606079858305));
#10440=CARTESIAN_POINT('Origin',(0.3,3.4,6.72));
#10441=CARTESIAN_POINT('',(0.3,3.5,6.72));
#10442=CARTESIAN_POINT('',(0.15,3.5,6.72));
#10443=CARTESIAN_POINT('',(0.3,6.5,6.72));
#10444=CARTESIAN_POINT('',(0.3,3.4,6.72));
#10445=CARTESIAN_POINT('',(0.15,6.5,6.72));
#10446=CARTESIAN_POINT('Origin',(0.3,3.4,8.));
#10447=CARTESIAN_POINT('',(0.3,3.5,7.04606079858305));
#10448=CARTESIAN_POINT('',(0.3,3.5,8.));
#10449=CARTESIAN_POINT('',(0.3,6.5,7.04606079858305));
#10450=CARTESIAN_POINT('',(0.3,3.5,7.04606079858305));
#10451=CARTESIAN_POINT('',(0.3,6.5,8.));
#10452=CARTESIAN_POINT('Origin',(0.,6.5,8.));
#10453=CARTESIAN_POINT('',(-6.,6.5,8.));
#10454=CARTESIAN_POINT('Origin',(0.,6.5,8.));
#10455=CARTESIAN_POINT('',(-2.58,6.5,4.10288568297003));
#10456=CARTESIAN_POINT('Origin',(-2.25,6.5,4.10288568297003));
#10457=CARTESIAN_POINT('',(4.17,6.5,8.));
#10458=CARTESIAN_POINT('Origin',(4.5,6.5,8.));
#10459=CARTESIAN_POINT('',(1.92,6.5,11.89711431703));
#10460=CARTESIAN_POINT('Origin',(2.25,6.5,11.89711431703));
#10461=CARTESIAN_POINT('',(-2.58,6.5,11.89711431703));
#10462=CARTESIAN_POINT('Origin',(-2.25,6.5,11.89711431703));
#10463=CARTESIAN_POINT('',(-4.83,6.5,8.));
#10464=CARTESIAN_POINT('Origin',(-4.5,6.5,8.));
#10465=CARTESIAN_POINT('',(1.92,6.5,4.10288568297003));
#10466=CARTESIAN_POINT('Origin',(2.25,6.5,4.10288568297003));
#10467=CARTESIAN_POINT('Origin',(0.,6.5,8.));
#10468=CARTESIAN_POINT('Origin',(0.,3.5,8.));
#10469=CARTESIAN_POINT('Origin',(0.,3.5,8.));
#10470=CARTESIAN_POINT('Origin',(-2.25,5.4,4.10288568297003));
#10471=CARTESIAN_POINT('',(-2.58,5.5,4.10288568297003));
#10472=CARTESIAN_POINT('Origin',(-2.25,5.5,4.10288568297003));
#10473=CARTESIAN_POINT('',(-2.58,5.4,4.10288568297003));
#10474=CARTESIAN_POINT('Origin',(4.5,5.4,8.));
#10475=CARTESIAN_POINT('',(4.17,5.5,8.));
#10476=CARTESIAN_POINT('Origin',(4.5,5.5,8.));
#10477=CARTESIAN_POINT('',(4.17,5.4,8.));
#10478=CARTESIAN_POINT('Origin',(2.25,5.4,11.89711431703));
#10479=CARTESIAN_POINT('',(1.92,5.5,11.89711431703));
#10480=CARTESIAN_POINT('Origin',(2.25,5.5,11.89711431703));
#10481=CARTESIAN_POINT('',(1.92,5.4,11.89711431703));
#10482=CARTESIAN_POINT('Origin',(-2.25,5.4,11.89711431703));
#10483=CARTESIAN_POINT('',(-2.58,5.5,11.89711431703));
#10484=CARTESIAN_POINT('Origin',(-2.25,5.5,11.89711431703));
#10485=CARTESIAN_POINT('',(-2.58,5.4,11.89711431703));
#10486=CARTESIAN_POINT('Origin',(-4.5,5.4,8.));
#10487=CARTESIAN_POINT('',(-4.83,5.5,8.));
#10488=CARTESIAN_POINT('Origin',(-4.5,5.5,8.));
#10489=CARTESIAN_POINT('',(-4.83,5.4,8.));
#10490=CARTESIAN_POINT('Origin',(2.25,5.4,4.10288568297003));
#10491=CARTESIAN_POINT('',(1.92,5.5,4.10288568297003));
#10492=CARTESIAN_POINT('Origin',(2.25,5.5,4.10288568297003));
#10493=CARTESIAN_POINT('',(1.92,5.4,4.10288568297003));
#10494=CARTESIAN_POINT('Origin',(0.,5.5,8.));
#10495=CARTESIAN_POINT('',(-6.,5.5,8.));
#10496=CARTESIAN_POINT('Origin',(0.,5.5,8.));
#10497=CARTESIAN_POINT('',(-1.8,5.5,8.));
#10498=CARTESIAN_POINT('Origin',(0.,5.5,8.));
#10499=CARTESIAN_POINT('Origin',(0.,5.5,8.));
#10500=CARTESIAN_POINT('',(-6.,5.5,8.));
#10501=CARTESIAN_POINT('Origin',(0.,3.5,8.));
#10502=CARTESIAN_POINT('',(-1.8,3.5,8.));
#10503=CARTESIAN_POINT('',(-1.8,3.5,8.));
#10504=CARTESIAN_POINT('Origin',(0.,3.5,8.));
#10505=CARTESIAN_POINT('Origin',(0.,3.5,8.));
#10506=CARTESIAN_POINT('',(0.,0.,0.));
#10507=CARTESIAN_POINT('Origin',(0.,6.5,8.));
#10508=CARTESIAN_POINT('',(-0.425,6.7,8.));
#10509=CARTESIAN_POINT('Origin',(0.,6.7,8.));
#10510=CARTESIAN_POINT('',(-0.425,6.5,8.));
#10511=CARTESIAN_POINT('',(-0.425,6.5,8.));
#10512=CARTESIAN_POINT('Origin',(0.,6.5,8.));
#10513=CARTESIAN_POINT('Origin',(0.,6.5,8.));
#10514=CARTESIAN_POINT('',(-1.4,6.7,8.));
#10515=CARTESIAN_POINT('Origin',(0.,6.7,8.));
#10516=CARTESIAN_POINT('',(-1.4,6.5,8.));
#10517=CARTESIAN_POINT('',(-1.4,6.5,8.));
#10518=CARTESIAN_POINT('Origin',(0.,6.5,8.));
#10519=CARTESIAN_POINT('Origin',(0.,6.7,8.));
#10520=CARTESIAN_POINT('Origin',(0.,6.5,8.));
#10521=CARTESIAN_POINT('',(0.,0.,0.));
#10522=CARTESIAN_POINT('Origin',(-0.2,-1.,-0.78));
#10523=CARTESIAN_POINT('',(-0.2,-0.9,-0.78));
#10524=CARTESIAN_POINT('',(-0.2,-0.9,-0.565685424949238));
#10525=CARTESIAN_POINT('',(-0.2,-0.9,-0.39));
#10526=CARTESIAN_POINT('',(-0.2,0.85,-0.78));
#10527=CARTESIAN_POINT('',(-0.2,-1.,-0.78));
#10528=CARTESIAN_POINT('',(-0.2,0.85,-0.565685424949238));
#10529=CARTESIAN_POINT('',(-0.2,0.85,-0.39));
#10530=CARTESIAN_POINT('',(-0.2,0.,-0.565685424949238));
#10531=CARTESIAN_POINT('Origin',(0.2,-1.,-0.78));
#10532=CARTESIAN_POINT('',(0.2,-0.9,-0.78));
#10533=CARTESIAN_POINT('',(0.1,-0.9,-0.78));
#10534=CARTESIAN_POINT('',(0.2,0.85,-0.78));
#10535=CARTESIAN_POINT('',(0.2,-1.,-0.78));
#10536=CARTESIAN_POINT('',(0.1,0.85,-0.78));
#10537=CARTESIAN_POINT('',(-0.125,-0.5,-0.78));
#10538=CARTESIAN_POINT('Origin',(0.,-0.5,-0.78));
#10539=CARTESIAN_POINT('Origin',(0.2,-1.,0.));
#10540=CARTESIAN_POINT('',(0.2,-0.9,-0.565685424949238));
#10541=CARTESIAN_POINT('',(0.2,-0.9,0.));
#10542=CARTESIAN_POINT('',(0.2,0.85,-0.565685424949238));
#10543=CARTESIAN_POINT('',(0.2,0.,-0.565685424949238));
#10544=CARTESIAN_POINT('',(0.2,0.85,0.));
#10545=CARTESIAN_POINT('Origin',(0.,0.85,0.));
#10546=CARTESIAN_POINT('',(-1.4,0.85,1.71450551880629E-16));
#10547=CARTESIAN_POINT('Origin',(0.,0.85,0.));
#10548=CARTESIAN_POINT('Origin',(0.,0.85,0.));
#10549=CARTESIAN_POINT('Origin',(0.,0.,0.));
#10550=CARTESIAN_POINT('Origin',(0.,-0.9,0.));
#10551=CARTESIAN_POINT('',(0.125,-0.5,0.586834729715275));
#10552=CARTESIAN_POINT('',(-0.125,-0.5,0.586834729715275));
#10553=CARTESIAN_POINT('Ctrl Pts',(0.125,-0.5,0.586834729715275));
#10554=CARTESIAN_POINT('Ctrl Pts',(0.125,-0.484254474936005,0.586834729715275));
#10555=CARTESIAN_POINT('Ctrl Pts',(0.121843784097853,-0.467492086231842,
0.587534197873268));
#10556=CARTESIAN_POINT('Ctrl Pts',(0.109073016834181,-0.436709004341607,
0.590038488226116));
#10557=CARTESIAN_POINT('Ctrl Pts',(0.0994608796208941,-0.422684184324257,
0.591804743154611));
#10558=CARTESIAN_POINT('Ctrl Pts',(0.077316548567853,-0.400539853271216,
0.59510289473619));
#10559=CARTESIAN_POINT('Ctrl Pts',(0.0632914182239686,-0.390927142361291,
0.596852269967858));
#10560=CARTESIAN_POINT('Ctrl Pts',(0.0325072544867634,-0.378155958502111,
0.599317707212167));
#10561=CARTESIAN_POINT('Ctrl Pts',(0.0157444828659572,-0.375,0.6));
#10562=CARTESIAN_POINT('Ctrl Pts',(-0.0157444828659573,-0.375,0.6));
#10563=CARTESIAN_POINT('Ctrl Pts',(-0.0325072544867634,-0.378155958502111,
0.599317707212167));
#10564=CARTESIAN_POINT('Ctrl Pts',(-0.0632914182239687,-0.390927142361291,
0.596852269967858));
#10565=CARTESIAN_POINT('Ctrl Pts',(-0.077316548567853,-0.400539853271216,
0.59510289473619));
#10566=CARTESIAN_POINT('Ctrl Pts',(-0.0994608796208942,-0.422684184324257,
0.591804743154611));
#10567=CARTESIAN_POINT('Ctrl Pts',(-0.109073016834181,-0.436709004341607,
0.590038488226116));
#10568=CARTESIAN_POINT('Ctrl Pts',(-0.121843784097853,-0.467492086231842,
0.587534197873268));
#10569=CARTESIAN_POINT('Ctrl Pts',(-0.125,-0.484254474936005,0.586834729715275));
#10570=CARTESIAN_POINT('Ctrl Pts',(-0.125,-0.5,0.586834729715275));
#10571=CARTESIAN_POINT('Ctrl Pts',(-0.125,-0.5,0.586834729715275));
#10572=CARTESIAN_POINT('Ctrl Pts',(-0.125,-0.515745525063995,0.586834729715275));
#10573=CARTESIAN_POINT('Ctrl Pts',(-0.121843784097853,-0.532507913768158,
0.587534197873268));
#10574=CARTESIAN_POINT('Ctrl Pts',(-0.109073016834181,-0.563290995658393,
0.590038488226116));
#10575=CARTESIAN_POINT('Ctrl Pts',(-0.0994608796208941,-0.577315815675743,
0.591804743154611));
#10576=CARTESIAN_POINT('Ctrl Pts',(-0.077316548567853,-0.599460146728784,
0.59510289473619));
#10577=CARTESIAN_POINT('Ctrl Pts',(-0.0632914182239687,-0.609072857638709,
0.596852269967858));
#10578=CARTESIAN_POINT('Ctrl Pts',(-0.0325072544867635,-0.621844041497889,
0.599317707212167));
#10579=CARTESIAN_POINT('Ctrl Pts',(-0.0157444828659572,-0.625,0.6));
#10580=CARTESIAN_POINT('Ctrl Pts',(0.0157444828659572,-0.625,0.6));
#10581=CARTESIAN_POINT('Ctrl Pts',(0.0325072544867633,-0.621844041497889,
0.599317707212167));
#10582=CARTESIAN_POINT('Ctrl Pts',(0.0632914182239686,-0.609072857638709,
0.596852269967858));
#10583=CARTESIAN_POINT('Ctrl Pts',(0.077316548567853,-0.599460146728784,
0.59510289473619));
#10584=CARTESIAN_POINT('Ctrl Pts',(0.0994608796208942,-0.577315815675743,
0.591804743154611));
#10585=CARTESIAN_POINT('Ctrl Pts',(0.109073016834181,-0.563290995658393,
0.590038488226116));
#10586=CARTESIAN_POINT('Ctrl Pts',(0.121843784097853,-0.532507913768158,
0.587534197873268));
#10587=CARTESIAN_POINT('Ctrl Pts',(0.125,-0.515745525063995,0.586834729715275));
#10588=CARTESIAN_POINT('Ctrl Pts',(0.125,-0.5,0.586834729715275));
#10589=CARTESIAN_POINT('',(-0.586834729715275,-0.5,-0.125));
#10590=CARTESIAN_POINT('',(-0.586834729715275,-0.5,0.125));
#10591=CARTESIAN_POINT('Ctrl Pts',(-0.586834729715275,-0.5,-0.125));
#10592=CARTESIAN_POINT('Ctrl Pts',(-0.586834729715275,-0.515745525063995,
-0.125));
#10593=CARTESIAN_POINT('Ctrl Pts',(-0.587534197873268,-0.532507913768158,
-0.121843784097853));
#10594=CARTESIAN_POINT('Ctrl Pts',(-0.590038488226116,-0.563290995658393,
-0.109073016834181));
#10595=CARTESIAN_POINT('Ctrl Pts',(-0.591804743154611,-0.577315815675743,
-0.0994608796208942));
#10596=CARTESIAN_POINT('Ctrl Pts',(-0.59510289473619,-0.599460146728784,
-0.0773165485678531));
#10597=CARTESIAN_POINT('Ctrl Pts',(-0.596852269967858,-0.609072857638709,
-0.0632914182239687));
#10598=CARTESIAN_POINT('Ctrl Pts',(-0.599317707212167,-0.621844041497889,
-0.0325072544867635));
#10599=CARTESIAN_POINT('Ctrl Pts',(-0.6,-0.625,-0.0157444828659573));
#10600=CARTESIAN_POINT('Ctrl Pts',(-0.6,-0.625,0.0157444828659572));
#10601=CARTESIAN_POINT('Ctrl Pts',(-0.599317707212167,-0.621844041497889,
0.0325072544867633));
#10602=CARTESIAN_POINT('Ctrl Pts',(-0.596852269967858,-0.609072857638709,
0.0632914182239686));
#10603=CARTESIAN_POINT('Ctrl Pts',(-0.59510289473619,-0.599460146728784,
0.077316548567853));
#10604=CARTESIAN_POINT('Ctrl Pts',(-0.591804743154611,-0.577315815675743,
0.0994608796208941));
#10605=CARTESIAN_POINT('Ctrl Pts',(-0.590038488226116,-0.563290995658393,
0.109073016834181));
#10606=CARTESIAN_POINT('Ctrl Pts',(-0.587534197873268,-0.532507913768158,
0.121843784097853));
#10607=CARTESIAN_POINT('Ctrl Pts',(-0.586834729715275,-0.515745525063995,
0.125));
#10608=CARTESIAN_POINT('Ctrl Pts',(-0.586834729715275,-0.5,0.125));
#10609=CARTESIAN_POINT('Ctrl Pts',(-0.586834729715275,-0.5,0.125));
#10610=CARTESIAN_POINT('Ctrl Pts',(-0.586834729715275,-0.484254474936005,
0.125));
#10611=CARTESIAN_POINT('Ctrl Pts',(-0.587534197873268,-0.467492086231842,
0.121843784097853));
#10612=CARTESIAN_POINT('Ctrl Pts',(-0.590038488226116,-0.436709004341607,
0.109073016834181));
#10613=CARTESIAN_POINT('Ctrl Pts',(-0.591804743154611,-0.422684184324257,
0.0994608796208941));
#10614=CARTESIAN_POINT('Ctrl Pts',(-0.59510289473619,-0.400539853271216,
0.077316548567853));
#10615=CARTESIAN_POINT('Ctrl Pts',(-0.596852269967858,-0.390927142361291,
0.0632914182239686));
#10616=CARTESIAN_POINT('Ctrl Pts',(-0.599317707212167,-0.378155958502111,
0.0325072544867634));
#10617=CARTESIAN_POINT('Ctrl Pts',(-0.6,-0.375,0.0157444828659572));
#10618=CARTESIAN_POINT('Ctrl Pts',(-0.6,-0.375,-0.0157444828659572));
#10619=CARTESIAN_POINT('Ctrl Pts',(-0.599317707212167,-0.378155958502111,
-0.0325072544867634));
#10620=CARTESIAN_POINT('Ctrl Pts',(-0.596852269967858,-0.390927142361291,
-0.0632914182239686));
#10621=CARTESIAN_POINT('Ctrl Pts',(-0.59510289473619,-0.400539853271216,
-0.077316548567853));
#10622=CARTESIAN_POINT('Ctrl Pts',(-0.591804743154611,-0.422684184324257,
-0.0994608796208942));
#10623=CARTESIAN_POINT('Ctrl Pts',(-0.590038488226116,-0.436709004341607,
-0.109073016834181));
#10624=CARTESIAN_POINT('Ctrl Pts',(-0.587534197873268,-0.467492086231842,
-0.121843784097853));
#10625=CARTESIAN_POINT('Ctrl Pts',(-0.586834729715275,-0.484254474936005,
-0.125));
#10626=CARTESIAN_POINT('Ctrl Pts',(-0.586834729715275,-0.5,-0.125));
#10627=CARTESIAN_POINT('',(0.586834729715275,-0.5,-0.125));
#10628=CARTESIAN_POINT('',(0.586834729715275,-0.5,0.125));
#10629=CARTESIAN_POINT('Ctrl Pts',(0.586834729715275,-0.5,-0.125));
#10630=CARTESIAN_POINT('Ctrl Pts',(0.586834729715275,-0.484254474936005,
-0.125));
#10631=CARTESIAN_POINT('Ctrl Pts',(0.587534197873268,-0.467492086231842,
-0.121843784097853));
#10632=CARTESIAN_POINT('Ctrl Pts',(0.590038488226116,-0.436709004341607,
-0.109073016834181));
#10633=CARTESIAN_POINT('Ctrl Pts',(0.591804743154611,-0.422684184324257,
-0.0994608796208941));
#10634=CARTESIAN_POINT('Ctrl Pts',(0.59510289473619,-0.400539853271216,
-0.0773165485678529));
#10635=CARTESIAN_POINT('Ctrl Pts',(0.596852269967858,-0.390927142361291,
-0.0632914182239686));
#10636=CARTESIAN_POINT('Ctrl Pts',(0.599317707212167,-0.378155958502111,
-0.0325072544867633));
#10637=CARTESIAN_POINT('Ctrl Pts',(0.6,-0.375,-0.0157444828659572));
#10638=CARTESIAN_POINT('Ctrl Pts',(0.6,-0.375,0.0157444828659573));
#10639=CARTESIAN_POINT('Ctrl Pts',(0.599317707212167,-0.378155958502111,
0.0325072544867635));
#10640=CARTESIAN_POINT('Ctrl Pts',(0.596852269967858,-0.390927142361291,
0.0632914182239687));
#10641=CARTESIAN_POINT('Ctrl Pts',(0.59510289473619,-0.400539853271216,
0.0773165485678531));
#10642=CARTESIAN_POINT('Ctrl Pts',(0.591804743154611,-0.422684184324257,
0.0994608796208942));
#10643=CARTESIAN_POINT('Ctrl Pts',(0.590038488226116,-0.436709004341607,
0.109073016834181));
#10644=CARTESIAN_POINT('Ctrl Pts',(0.587534197873268,-0.467492086231842,
0.121843784097853));
#10645=CARTESIAN_POINT('Ctrl Pts',(0.586834729715275,-0.484254474936005,
0.125));
#10646=CARTESIAN_POINT('Ctrl Pts',(0.586834729715275,-0.5,0.125));
#10647=CARTESIAN_POINT('Ctrl Pts',(0.586834729715275,-0.5,0.125));
#10648=CARTESIAN_POINT('Ctrl Pts',(0.586834729715275,-0.515745525063995,
0.125));
#10649=CARTESIAN_POINT('Ctrl Pts',(0.587534197873268,-0.532507913768158,
0.121843784097853));
#10650=CARTESIAN_POINT('Ctrl Pts',(0.590038488226116,-0.563290995658393,
0.109073016834181));
#10651=CARTESIAN_POINT('Ctrl Pts',(0.591804743154611,-0.577315815675743,
0.0994608796208942));
#10652=CARTESIAN_POINT('Ctrl Pts',(0.59510289473619,-0.599460146728784,
0.077316548567853));
#10653=CARTESIAN_POINT('Ctrl Pts',(0.596852269967858,-0.609072857638709,
0.0632914182239688));
#10654=CARTESIAN_POINT('Ctrl Pts',(0.599317707212167,-0.621844041497889,
0.0325072544867635));
#10655=CARTESIAN_POINT('Ctrl Pts',(0.6,-0.625,0.0157444828659573));
#10656=CARTESIAN_POINT('Ctrl Pts',(0.6,-0.625,-0.0157444828659572));
#10657=CARTESIAN_POINT('Ctrl Pts',(0.599317707212167,-0.621844041497889,
-0.0325072544867633));
#10658=CARTESIAN_POINT('Ctrl Pts',(0.596852269967858,-0.609072857638709,
-0.0632914182239685));
#10659=CARTESIAN_POINT('Ctrl Pts',(0.59510289473619,-0.599460146728784,
-0.077316548567853));
#10660=CARTESIAN_POINT('Ctrl Pts',(0.591804743154611,-0.577315815675743,
-0.0994608796208941));
#10661=CARTESIAN_POINT('Ctrl Pts',(0.590038488226116,-0.563290995658393,
-0.10907301683418));
#10662=CARTESIAN_POINT('Ctrl Pts',(0.587534197873268,-0.532507913768158,
-0.121843784097853));
#10663=CARTESIAN_POINT('Ctrl Pts',(0.586834729715275,-0.515745525063995,
-0.125));
#10664=CARTESIAN_POINT('Ctrl Pts',(0.586834729715275,-0.5,-0.125));
#10665=CARTESIAN_POINT('Origin',(0.,-0.5,0.));
#10666=CARTESIAN_POINT('',(-1.,-0.375,-6.12323399573677E-17));
#10667=CARTESIAN_POINT('',(-0.992156741649222,-0.5,0.125));
#10668=CARTESIAN_POINT('Ctrl Pts',(-1.,-0.375,-1.00613961606655E-16));
#10669=CARTESIAN_POINT('Ctrl Pts',(-1.,-0.375,0.0157128711428661));
#10670=CARTESIAN_POINT('Ctrl Pts',(-0.999591823858855,-0.378143583103513,
0.0324619190698278));
#10671=CARTESIAN_POINT('Ctrl Pts',(-0.998116453123232,-0.390905426591754,
0.0632545375991437));
#10672=CARTESIAN_POINT('Ctrl Pts',(-0.997070068816062,-0.400522781657727,
0.0772994769543643));
#10673=CARTESIAN_POINT('Ctrl Pts',(-0.995102104277285,-0.422700615683787,
0.0994773109804239));
#10674=CARTESIAN_POINT('Ctrl Pts',(-0.994052129228928,-0.436745514765346,
0.109094593469654));
#10675=CARTESIAN_POINT('Ctrl Pts',(-0.99256853061881,-0.467537996927464,
0.121856383722779));
#10676=CARTESIAN_POINT('Ctrl Pts',(-0.992156741649222,-0.484286997589363,
0.125));
#10677=CARTESIAN_POINT('Ctrl Pts',(-0.992156741649222,-0.5,0.125));
#10678=CARTESIAN_POINT('',(-1.,-0.625,-6.12323399573677E-17));
#10679=CARTESIAN_POINT('Ctrl Pts',(-1.,-0.625,-4.5102810375397E-17));
#10680=CARTESIAN_POINT('Ctrl Pts',(-1.,-0.625,-0.0157128711428662));
#10681=CARTESIAN_POINT('Ctrl Pts',(-0.999591823858855,-0.621856416896487,
-0.032461919069828));
#10682=CARTESIAN_POINT('Ctrl Pts',(-0.998116453123232,-0.609094573408246,
-0.0632545375991439));
#10683=CARTESIAN_POINT('Ctrl Pts',(-0.997070068816062,-0.599477218342273,
-0.0772994769543645));
#10684=CARTESIAN_POINT('Ctrl Pts',(-0.995102104277285,-0.577299384316213,
-0.0994773109804241));
#10685=CARTESIAN_POINT('Ctrl Pts',(-0.994052129228928,-0.563254485234654,
-0.109094593469655));
#10686=CARTESIAN_POINT('Ctrl Pts',(-0.99256853061881,-0.532462003072536,
-0.121856383722779));
#10687=CARTESIAN_POINT('Ctrl Pts',(-0.992156741649221,-0.515713002410637,
-0.125));
#10688=CARTESIAN_POINT('Ctrl Pts',(-0.992156741649221,-0.484286997589363,
-0.125));
#10689=CARTESIAN_POINT('Ctrl Pts',(-0.99256853061881,-0.467537996927464,
-0.121856383722779));
#10690=CARTESIAN_POINT('Ctrl Pts',(-0.994052129228928,-0.436745514765346,
-0.109094593469655));
#10691=CARTESIAN_POINT('Ctrl Pts',(-0.995102104277285,-0.422700615683787,
-0.0994773109804241));
#10692=CARTESIAN_POINT('Ctrl Pts',(-0.997070068816062,-0.400522781657728,
-0.0772994769543645));
#10693=CARTESIAN_POINT('Ctrl Pts',(-0.998116453123232,-0.390905426591754,
-0.063254537599144));
#10694=CARTESIAN_POINT('Ctrl Pts',(-0.999591823858855,-0.378143583103513,
-0.0324619190698281));
#10695=CARTESIAN_POINT('Ctrl Pts',(-1.,-0.375,-0.0157128711428663));
#10696=CARTESIAN_POINT('Ctrl Pts',(-1.,-0.375,-9.36750677027476E-17));
#10697=CARTESIAN_POINT('Ctrl Pts',(-0.992156741649222,-0.5,0.125));
#10698=CARTESIAN_POINT('Ctrl Pts',(-0.992156741649222,-0.515713002410637,
0.125));
#10699=CARTESIAN_POINT('Ctrl Pts',(-0.99256853061881,-0.532462003072536,
0.121856383722779));
#10700=CARTESIAN_POINT('Ctrl Pts',(-0.994052129228928,-0.563254485234654,
0.109094593469654));
#10701=CARTESIAN_POINT('Ctrl Pts',(-0.995102104277285,-0.577299384316213,
0.0994773109804241));
#10702=CARTESIAN_POINT('Ctrl Pts',(-0.997070068816062,-0.599477218342273,
0.0772994769543644));
#10703=CARTESIAN_POINT('Ctrl Pts',(-0.998116453123232,-0.609094573408246,
0.0632545375991438));
#10704=CARTESIAN_POINT('Ctrl Pts',(-0.999591823858855,-0.621856416896487,
0.0324619190698279));
#10705=CARTESIAN_POINT('Ctrl Pts',(-1.,-0.625,0.0157128711428661));
#10706=CARTESIAN_POINT('Ctrl Pts',(-1.,-0.625,-4.85722573273506E-17));
#10707=CARTESIAN_POINT('',(-7.65404249467096E-18,-0.5,0.125));
#10708=CARTESIAN_POINT('Origin',(0.,-0.5,0.));
#10709=CARTESIAN_POINT('',(0.992156741649222,-0.5,0.125));
#10710=CARTESIAN_POINT('',(-7.65404249467096E-18,-0.5,0.125));
#10711=CARTESIAN_POINT('',(1.,-0.625,6.12323399573677E-17));
#10712=CARTESIAN_POINT('Ctrl Pts',(1.,-0.625,7.28583859910259E-17));
#10713=CARTESIAN_POINT('Ctrl Pts',(1.,-0.625,0.0157128711428663));
#10714=CARTESIAN_POINT('Ctrl Pts',(0.999591823858855,-0.621856416896487,
0.032461919069828));
#10715=CARTESIAN_POINT('Ctrl Pts',(0.998116453123232,-0.609094573408246,
0.0632545375991439));
#10716=CARTESIAN_POINT('Ctrl Pts',(0.997070068816062,-0.599477218342273,
0.0772994769543645));
#10717=CARTESIAN_POINT('Ctrl Pts',(0.995102104277285,-0.577299384316213,
0.0994773109804242));
#10718=CARTESIAN_POINT('Ctrl Pts',(0.994052129228928,-0.563254485234654,
0.109094593469655));
#10719=CARTESIAN_POINT('Ctrl Pts',(0.99256853061881,-0.532462003072536,
0.121856383722779));
#10720=CARTESIAN_POINT('Ctrl Pts',(0.992156741649222,-0.515713002410637,
0.125));
#10721=CARTESIAN_POINT('Ctrl Pts',(0.992156741649222,-0.5,0.125));
#10722=CARTESIAN_POINT('',(1.,-0.375,6.12323399573677E-17));
#10723=CARTESIAN_POINT('Ctrl Pts',(1.,-0.375,2.08166817117217E-17));
#10724=CARTESIAN_POINT('Ctrl Pts',(1.,-0.375,-0.0157128711428662));
#10725=CARTESIAN_POINT('Ctrl Pts',(0.999591823858855,-0.378143583103513,
-0.032461919069828));
#10726=CARTESIAN_POINT('Ctrl Pts',(0.998116453123232,-0.390905426591754,
-0.0632545375991438));
#10727=CARTESIAN_POINT('Ctrl Pts',(0.997070068816062,-0.400522781657728,
-0.0772994769543644));
#10728=CARTESIAN_POINT('Ctrl Pts',(0.995102104277285,-0.422700615683787,
-0.099477310980424));
#10729=CARTESIAN_POINT('Ctrl Pts',(0.994052129228928,-0.436745514765346,
-0.109094593469654));
#10730=CARTESIAN_POINT('Ctrl Pts',(0.99256853061881,-0.467537996927464,
-0.121856383722779));
#10731=CARTESIAN_POINT('Ctrl Pts',(0.992156741649222,-0.484286997589363,
-0.125));
#10732=CARTESIAN_POINT('Ctrl Pts',(0.992156741649222,-0.515713002410637,
-0.125));
#10733=CARTESIAN_POINT('Ctrl Pts',(0.99256853061881,-0.532462003072536,
-0.121856383722779));
#10734=CARTESIAN_POINT('Ctrl Pts',(0.994052129228928,-0.563254485234654,
-0.109094593469654));
#10735=CARTESIAN_POINT('Ctrl Pts',(0.995102104277285,-0.577299384316213,
-0.099477310980424));
#10736=CARTESIAN_POINT('Ctrl Pts',(0.997070068816062,-0.599477218342273,
-0.0772994769543643));
#10737=CARTESIAN_POINT('Ctrl Pts',(0.998116453123232,-0.609094573408246,
-0.0632545375991438));
#10738=CARTESIAN_POINT('Ctrl Pts',(0.999591823858855,-0.621856416896487,
-0.0324619190698279));
#10739=CARTESIAN_POINT('Ctrl Pts',(1.,-0.625,-0.0157128711428661));
#10740=CARTESIAN_POINT('Ctrl Pts',(1.,-0.625,8.32667268468867E-17));
#10741=CARTESIAN_POINT('Ctrl Pts',(0.992156741649222,-0.5,0.125));
#10742=CARTESIAN_POINT('Ctrl Pts',(0.992156741649222,-0.484286997589363,
0.125));
#10743=CARTESIAN_POINT('Ctrl Pts',(0.99256853061881,-0.467537996927464,
0.121856383722779));
#10744=CARTESIAN_POINT('Ctrl Pts',(0.994052129228928,-0.436745514765346,
0.109094593469654));
#10745=CARTESIAN_POINT('Ctrl Pts',(0.995102104277285,-0.422700615683787,
0.0994773109804241));
#10746=CARTESIAN_POINT('Ctrl Pts',(0.997070068816062,-0.400522781657727,
0.0772994769543644));
#10747=CARTESIAN_POINT('Ctrl Pts',(0.998116453123232,-0.390905426591754,
0.0632545375991438));
#10748=CARTESIAN_POINT('Ctrl Pts',(0.999591823858855,-0.378143583103513,
0.0324619190698279));
#10749=CARTESIAN_POINT('Ctrl Pts',(1.,-0.375,0.0157128711428662));
#10750=CARTESIAN_POINT('Ctrl Pts',(1.,-0.375,2.77555756156289E-17));
#10751=CARTESIAN_POINT('Origin',(0.,-0.1,0.));
#10752=CARTESIAN_POINT('',(-1.,-0.9,1.22464679914735E-16));
#10753=CARTESIAN_POINT('Origin',(0.,-0.9,0.));
#10754=CARTESIAN_POINT('',(-1.,-0.1,-1.22464679914735E-16));
#10755=CARTESIAN_POINT('',(-1.,-0.1,1.22464679914735E-16));
#10756=CARTESIAN_POINT('',(-1.,-0.1,-1.22464679914735E-16));
#10757=CARTESIAN_POINT('Origin',(0.,-0.1,0.));
#10758=CARTESIAN_POINT('',(0.,-0.625,-1.));
#10759=CARTESIAN_POINT('',(0.,-0.375,-1.));
#10760=CARTESIAN_POINT('Ctrl Pts',(-2.08166817117217E-17,-0.625,-1.));
#10761=CARTESIAN_POINT('Ctrl Pts',(0.0157128711428662,-0.625,-1.));
#10762=CARTESIAN_POINT('Ctrl Pts',(0.0324619190698279,-0.621856416896487,
-0.999591823858855));
#10763=CARTESIAN_POINT('Ctrl Pts',(0.0632545375991438,-0.609094573408246,
-0.998116453123232));
#10764=CARTESIAN_POINT('Ctrl Pts',(0.0772994769543644,-0.599477218342273,
-0.997070068816062));
#10765=CARTESIAN_POINT('Ctrl Pts',(0.0994773109804241,-0.577299384316213,
-0.995102104277285));
#10766=CARTESIAN_POINT('Ctrl Pts',(0.109094593469654,-0.563254485234654,
-0.994052129228928));
#10767=CARTESIAN_POINT('Ctrl Pts',(0.121856383722779,-0.532462003072536,
-0.99256853061881));
#10768=CARTESIAN_POINT('Ctrl Pts',(0.125,-0.515713002410637,-0.992156741649221));
#10769=CARTESIAN_POINT('Ctrl Pts',(0.125,-0.484286997589363,-0.992156741649221));
#10770=CARTESIAN_POINT('Ctrl Pts',(0.121856383722779,-0.467537996927464,
-0.99256853061881));
#10771=CARTESIAN_POINT('Ctrl Pts',(0.109094593469654,-0.436745514765346,
-0.994052129228928));
#10772=CARTESIAN_POINT('Ctrl Pts',(0.0994773109804241,-0.422700615683787,
-0.995102104277285));
#10773=CARTESIAN_POINT('Ctrl Pts',(0.0772994769543645,-0.400522781657728,
-0.997070068816062));
#10774=CARTESIAN_POINT('Ctrl Pts',(0.0632545375991439,-0.390905426591754,
-0.998116453123232));
#10775=CARTESIAN_POINT('Ctrl Pts',(0.032461919069828,-0.378143583103513,
-0.999591823858855));
#10776=CARTESIAN_POINT('Ctrl Pts',(0.0157128711428662,-0.375,-1.));
#10777=CARTESIAN_POINT('Ctrl Pts',(3.81639164714898E-17,-0.375,-1.));
#10778=CARTESIAN_POINT('',(-0.125,-0.5,-0.992156741649222));
#10779=CARTESIAN_POINT('Ctrl Pts',(4.5102810375397E-17,-0.375,-1.));
#10780=CARTESIAN_POINT('Ctrl Pts',(-0.0157128711428661,-0.375,-1.));
#10781=CARTESIAN_POINT('Ctrl Pts',(-0.0324619190698279,-0.378143583103513,
-0.999591823858855));
#10782=CARTESIAN_POINT('Ctrl Pts',(-0.0632545375991437,-0.390905426591754,
-0.998116453123232));
#10783=CARTESIAN_POINT('Ctrl Pts',(-0.0772994769543643,-0.400522781657727,
-0.997070068816062));
#10784=CARTESIAN_POINT('Ctrl Pts',(-0.099477310980424,-0.422700615683787,
-0.995102104277285));
#10785=CARTESIAN_POINT('Ctrl Pts',(-0.109094593469654,-0.436745514765346,
-0.994052129228928));
#10786=CARTESIAN_POINT('Ctrl Pts',(-0.121856383722779,-0.467537996927464,
-0.99256853061881));
#10787=CARTESIAN_POINT('Ctrl Pts',(-0.125,-0.484286997589363,-0.992156741649222));
#10788=CARTESIAN_POINT('Ctrl Pts',(-0.125,-0.5,-0.992156741649222));
#10789=CARTESIAN_POINT('Ctrl Pts',(-0.125,-0.5,-0.992156741649222));
#10790=CARTESIAN_POINT('Ctrl Pts',(-0.125,-0.515713002410637,-0.992156741649222));
#10791=CARTESIAN_POINT('Ctrl Pts',(-0.121856383722779,-0.532462003072536,
-0.99256853061881));
#10792=CARTESIAN_POINT('Ctrl Pts',(-0.109094593469654,-0.563254485234654,
-0.994052129228928));
#10793=CARTESIAN_POINT('Ctrl Pts',(-0.0994773109804241,-0.577299384316213,
-0.995102104277285));
#10794=CARTESIAN_POINT('Ctrl Pts',(-0.0772994769543644,-0.599477218342273,
-0.997070068816062));
#10795=CARTESIAN_POINT('Ctrl Pts',(-0.0632545375991439,-0.609094573408246,
-0.998116453123232));
#10796=CARTESIAN_POINT('Ctrl Pts',(-0.032461919069828,-0.621856416896487,
-0.999591823858855));
#10797=CARTESIAN_POINT('Ctrl Pts',(-0.0157128711428662,-0.625,-1.));
#10798=CARTESIAN_POINT('Ctrl Pts',(-1.38777878078145E-17,-0.625,-1.));
#10799=CARTESIAN_POINT('',(0.,-0.375,1.));
#10800=CARTESIAN_POINT('',(0.,-0.625,1.));
#10801=CARTESIAN_POINT('Ctrl Pts',(4.16333634234434E-17,-0.375,1.));
#10802=CARTESIAN_POINT('Ctrl Pts',(0.0157128711428662,-0.375,1.));
#10803=CARTESIAN_POINT('Ctrl Pts',(0.032461919069828,-0.378143583103513,
0.999591823858855));
#10804=CARTESIAN_POINT('Ctrl Pts',(0.0632545375991439,-0.390905426591754,
0.998116453123232));
#10805=CARTESIAN_POINT('Ctrl Pts',(0.0772994769543644,-0.400522781657728,
0.997070068816062));
#10806=CARTESIAN_POINT('Ctrl Pts',(0.0994773109804241,-0.422700615683787,
0.995102104277285));
#10807=CARTESIAN_POINT('Ctrl Pts',(0.109094593469654,-0.436745514765346,
0.994052129228928));
#10808=CARTESIAN_POINT('Ctrl Pts',(0.121856383722779,-0.467537996927464,
0.99256853061881));
#10809=CARTESIAN_POINT('Ctrl Pts',(0.125,-0.484286997589363,0.992156741649222));
#10810=CARTESIAN_POINT('Ctrl Pts',(0.125,-0.515713002410637,0.992156741649222));
#10811=CARTESIAN_POINT('Ctrl Pts',(0.121856383722779,-0.532462003072536,
0.99256853061881));
#10812=CARTESIAN_POINT('Ctrl Pts',(0.109094593469655,-0.563254485234654,
0.994052129228928));
#10813=CARTESIAN_POINT('Ctrl Pts',(0.0994773109804241,-0.577299384316213,
0.995102104277285));
#10814=CARTESIAN_POINT('Ctrl Pts',(0.0772994769543644,-0.599477218342273,
0.997070068816062));
#10815=CARTESIAN_POINT('Ctrl Pts',(0.0632545375991438,-0.609094573408246,
0.998116453123232));
#10816=CARTESIAN_POINT('Ctrl Pts',(0.0324619190698279,-0.621856416896487,
0.999591823858855));
#10817=CARTESIAN_POINT('Ctrl Pts',(0.0157128711428662,-0.625,1.));
#10818=CARTESIAN_POINT('Ctrl Pts',(-1.73472347597681E-17,-0.625,1.));
#10819=CARTESIAN_POINT('',(-0.125,-0.5,0.992156741649222));
#10820=CARTESIAN_POINT('Ctrl Pts',(-1.73472347597681E-17,-0.625,1.));
#10821=CARTESIAN_POINT('Ctrl Pts',(-0.0157128711428662,-0.625,1.));
#10822=CARTESIAN_POINT('Ctrl Pts',(-0.032461919069828,-0.621856416896487,
0.999591823858855));
#10823=CARTESIAN_POINT('Ctrl Pts',(-0.0632545375991439,-0.609094573408246,
0.998116453123232));
#10824=CARTESIAN_POINT('Ctrl Pts',(-0.0772994769543645,-0.599477218342273,
0.997070068816062));
#10825=CARTESIAN_POINT('Ctrl Pts',(-0.0994773109804241,-0.577299384316213,
0.995102104277285));
#10826=CARTESIAN_POINT('Ctrl Pts',(-0.109094593469654,-0.563254485234654,
0.994052129228928));
#10827=CARTESIAN_POINT('Ctrl Pts',(-0.121856383722779,-0.532462003072536,
0.99256853061881));
#10828=CARTESIAN_POINT('Ctrl Pts',(-0.125,-0.515713002410637,0.992156741649222));
#10829=CARTESIAN_POINT('Ctrl Pts',(-0.125,-0.5,0.992156741649222));
#10830=CARTESIAN_POINT('Ctrl Pts',(-0.125,-0.5,0.992156741649222));
#10831=CARTESIAN_POINT('Ctrl Pts',(-0.125,-0.484286997589363,0.992156741649222));
#10832=CARTESIAN_POINT('Ctrl Pts',(-0.121856383722779,-0.467537996927464,
0.99256853061881));
#10833=CARTESIAN_POINT('Ctrl Pts',(-0.109094593469654,-0.436745514765346,
0.994052129228928));
#10834=CARTESIAN_POINT('Ctrl Pts',(-0.099477310980424,-0.422700615683787,
0.995102104277285));
#10835=CARTESIAN_POINT('Ctrl Pts',(-0.0772994769543643,-0.400522781657727,
0.997070068816062));
#10836=CARTESIAN_POINT('Ctrl Pts',(-0.0632545375991438,-0.390905426591754,
0.998116453123232));
#10837=CARTESIAN_POINT('Ctrl Pts',(-0.0324619190698279,-0.378143583103513,
0.999591823858855));
#10838=CARTESIAN_POINT('Ctrl Pts',(-0.0157128711428661,-0.375,1.));
#10839=CARTESIAN_POINT('Ctrl Pts',(4.5102810375397E-17,-0.375,1.));
#10840=CARTESIAN_POINT('Origin',(0.,-0.5,0.));
#10841=CARTESIAN_POINT('',(-0.125,-0.5,0.));
#10842=CARTESIAN_POINT('Origin',(0.,-0.5,0.));
#10843=CARTESIAN_POINT('',(-0.125,-0.5,0.));
#10844=CARTESIAN_POINT('Origin',(0.,-0.9,0.));
#10845=CARTESIAN_POINT('Origin',(0.,0.,0.));
#10846=CARTESIAN_POINT('',(-1.4,0.,1.71450551880629E-16));
#10847=CARTESIAN_POINT('Origin',(0.,0.,0.));
#10848=CARTESIAN_POINT('',(1.23958209161204,0.,0.143317017690053));
#10849=CARTESIAN_POINT('',(1.22320001975977,0.,0.246749348660852));
#10850=CARTESIAN_POINT('Origin',(1.21321664662686,0.,0.192154639568406));
#10851=CARTESIAN_POINT('',(1.20190105810224,0.,0.335465908756113));
#10852=CARTESIAN_POINT('Origin',(0.,0.,0.));
#10853=CARTESIAN_POINT('',(1.16954029537568,0.,0.435062095450087));
#10854=CARTESIAN_POINT('Origin',(1.1682203282434,0.,0.379577794185952));
#10855=CARTESIAN_POINT('',(1.13462523166105,0.,0.519354515801077));
#10856=CARTESIAN_POINT('Origin',(0.,0.,0.));
#10857=CARTESIAN_POINT('',(1.08708260743774,0.,0.612662169561029));
#10858=CARTESIAN_POINT('Origin',(1.0944585482776,0.,0.557654483764164));
#10859=CARTESIAN_POINT('',(1.0394111664111,0.,0.690454891028201));
#10860=CARTESIAN_POINT('Origin',(0.,0.,0.));
#10861=CARTESIAN_POINT('',(0.977857337884349,0.,0.775176467748211));
#10862=CARTESIAN_POINT('Origin',(0.993747566553533,0.,0.72199986920298));
#10863=CARTESIAN_POINT('',(0.918603348636233,0.,0.844553975349804));
#10864=CARTESIAN_POINT('Origin',(0.,0.,0.));
#10865=CARTESIAN_POINT('',(0.844553975349804,0.,0.918603348636233));
#10866=CARTESIAN_POINT('Origin',(0.86856722168183,0.,0.86856722168183));
#10867=CARTESIAN_POINT('',(0.775176467748211,0.,0.977857337884349));
#10868=CARTESIAN_POINT('Origin',(0.,0.,0.));
#10869=CARTESIAN_POINT('',(0.690454891028201,0.,1.0394111664111));
#10870=CARTESIAN_POINT('Origin',(0.721999869202979,0.,0.993747566553533));
#10871=CARTESIAN_POINT('',(0.612662169561028,0.,1.08708260743774));
#10872=CARTESIAN_POINT('Origin',(0.,0.,0.));
#10873=CARTESIAN_POINT('',(0.519354515801077,0.,1.13462523166105));
#10874=CARTESIAN_POINT('Origin',(0.557654483764164,0.,1.0944585482776));
#10875=CARTESIAN_POINT('',(0.435062095450087,0.,1.16954029537568));
#10876=CARTESIAN_POINT('Origin',(0.,0.,0.));
#10877=CARTESIAN_POINT('',(0.335465908756113,0.,1.20190105810224));
#10878=CARTESIAN_POINT('Origin',(0.379577794185951,0.,1.1682203282434));
#10879=CARTESIAN_POINT('',(0.246749348660851,0.,1.22320001975977));
#10880=CARTESIAN_POINT('Origin',(0.,0.,0.));
#10881=CARTESIAN_POINT('',(0.143317017690053,0.,1.23958209161204));
#10882=CARTESIAN_POINT('Origin',(0.192154639568406,0.,1.21321664662686));
#10883=CARTESIAN_POINT('',(0.0523608139934478,0.,1.24674050008925));
#10884=CARTESIAN_POINT('Origin',(0.,0.,0.));
#10885=CARTESIAN_POINT('',(-0.0523608139934483,0.,1.24674050008925));
#10886=CARTESIAN_POINT('Origin',(-2.25642313758905E-16,0.,1.22833954473516));
#10887=CARTESIAN_POINT('',(-0.143317017690053,0.,1.23958209161204));
#10888=CARTESIAN_POINT('Origin',(0.,0.,0.));
#10889=CARTESIAN_POINT('',(-0.246749348660852,0.,1.22320001975977));
#10890=CARTESIAN_POINT('Origin',(-0.192154639568406,0.,1.21321664662686));
#10891=CARTESIAN_POINT('',(-0.335465908756113,0.,1.20190105810224));
#10892=CARTESIAN_POINT('Origin',(0.,0.,0.));
#10893=CARTESIAN_POINT('',(-0.435062095450087,0.,1.16954029537568));
#10894=CARTESIAN_POINT('Origin',(-0.379577794185951,0.,1.1682203282434));
#10895=CARTESIAN_POINT('',(-0.519354515801077,0.,1.13462523166105));
#10896=CARTESIAN_POINT('Origin',(0.,0.,0.));
#10897=CARTESIAN_POINT('',(-0.612662169561029,0.,1.08708260743774));
#10898=CARTESIAN_POINT('Origin',(-0.557654483764164,0.,1.0944585482776));
#10899=CARTESIAN_POINT('',(-0.690454891028201,0.,1.0394111664111));
#10900=CARTESIAN_POINT('Origin',(0.,0.,0.));
#10901=CARTESIAN_POINT('',(-0.775176467748211,0.,0.977857337884349));
#10902=CARTESIAN_POINT('Origin',(-0.721999869202979,0.,0.993747566553533));
#10903=CARTESIAN_POINT('',(-0.844553975349804,0.,0.918603348636233));
#10904=CARTESIAN_POINT('Origin',(0.,0.,0.));
#10905=CARTESIAN_POINT('',(-0.918603348636233,0.,0.844553975349804));
#10906=CARTESIAN_POINT('Origin',(-0.86856722168183,0.,0.86856722168183));
#10907=CARTESIAN_POINT('',(-0.977857337884348,0.,0.775176467748211));
#10908=CARTESIAN_POINT('Origin',(0.,0.,0.));
#10909=CARTESIAN_POINT('',(-1.0394111664111,0.,0.690454891028201));
#10910=CARTESIAN_POINT('Origin',(-0.993747566553533,0.,0.721999869202979));
#10911=CARTESIAN_POINT('',(-1.08708260743774,0.,0.612662169561028));
#10912=CARTESIAN_POINT('Origin',(0.,0.,0.));
#10913=CARTESIAN_POINT('',(-1.13462523166105,0.,0.519354515801077));
#10914=CARTESIAN_POINT('Origin',(-1.0944585482776,0.,0.557654483764164));
#10915=CARTESIAN_POINT('',(-1.16954029537568,0.,0.435062095450087));
#10916=CARTESIAN_POINT('Origin',(0.,0.,0.));
#10917=CARTESIAN_POINT('',(-1.20190105810224,0.,0.335465908756113));
#10918=CARTESIAN_POINT('Origin',(-1.1682203282434,0.,0.379577794185951));
#10919=CARTESIAN_POINT('',(-1.22320001975977,0.,0.246749348660851));
#10920=CARTESIAN_POINT('Origin',(0.,0.,0.));
#10921=CARTESIAN_POINT('',(-1.23958209161204,0.,0.143317017690053));
#10922=CARTESIAN_POINT('Origin',(-1.21321664662686,0.,0.192154639568406));
#10923=CARTESIAN_POINT('',(-1.24674050008925,0.,0.0523608139934479));
#10924=CARTESIAN_POINT('Origin',(0.,0.,0.));
#10925=CARTESIAN_POINT('',(-1.24674050008925,0.,-0.0523608139934482));
#10926=CARTESIAN_POINT('Origin',(-1.22833954473516,0.,-1.50428209172603E-16));
#10927=CARTESIAN_POINT('',(-1.23958209161204,0.,-0.143317017690053));
#10928=CARTESIAN_POINT('Origin',(0.,0.,0.));
#10929=CARTESIAN_POINT('',(-1.22320001975977,0.,-0.246749348660852));
#10930=CARTESIAN_POINT('Origin',(-1.21321664662686,0.,-0.192154639568406));
#10931=CARTESIAN_POINT('',(-1.20190105810224,0.,-0.335465908756113));
#10932=CARTESIAN_POINT('Origin',(0.,0.,0.));
#10933=CARTESIAN_POINT('',(-1.16954029537568,0.,-0.435062095450087));
#10934=CARTESIAN_POINT('Origin',(-1.1682203282434,0.,-0.379577794185951));
#10935=CARTESIAN_POINT('',(-1.13462523166105,0.,-0.519354515801077));
#10936=CARTESIAN_POINT('Origin',(0.,0.,0.));
#10937=CARTESIAN_POINT('',(-1.08708260743774,0.,-0.612662169561029));
#10938=CARTESIAN_POINT('Origin',(-1.0944585482776,0.,-0.557654483764164));
#10939=CARTESIAN_POINT('',(-1.0394111664111,0.,-0.690454891028201));
#10940=CARTESIAN_POINT('Origin',(0.,0.,0.));
#10941=CARTESIAN_POINT('',(-0.977857337884349,0.,-0.775176467748211));
#10942=CARTESIAN_POINT('Origin',(-0.993747566553533,0.,-0.721999869202979));
#10943=CARTESIAN_POINT('',(-0.918603348636233,0.,-0.844553975349804));
#10944=CARTESIAN_POINT('Origin',(0.,0.,0.));
#10945=CARTESIAN_POINT('',(-0.844553975349804,0.,-0.918603348636233));
#10946=CARTESIAN_POINT('Origin',(-0.86856722168183,0.,-0.86856722168183));
#10947=CARTESIAN_POINT('',(-0.775176467748211,0.,-0.977857337884348));
#10948=CARTESIAN_POINT('Origin',(0.,0.,0.));
#10949=CARTESIAN_POINT('',(-0.690454891028201,0.,-1.0394111664111));
#10950=CARTESIAN_POINT('Origin',(-0.721999869202979,0.,-0.993747566553533));
#10951=CARTESIAN_POINT('',(-0.612662169561028,0.,-1.08708260743774));
#10952=CARTESIAN_POINT('Origin',(0.,0.,0.));
#10953=CARTESIAN_POINT('',(-0.519354515801077,0.,-1.13462523166105));
#10954=CARTESIAN_POINT('Origin',(-0.557654483764164,0.,-1.0944585482776));
#10955=CARTESIAN_POINT('',(-0.435062095450087,0.,-1.16954029537568));
#10956=CARTESIAN_POINT('Origin',(0.,0.,0.));
#10957=CARTESIAN_POINT('',(-0.335465908756113,0.,-1.20190105810224));
#10958=CARTESIAN_POINT('Origin',(-0.379577794185951,0.,-1.1682203282434));
#10959=CARTESIAN_POINT('',(-0.246749348660852,0.,-1.22320001975977));
#10960=CARTESIAN_POINT('Origin',(0.,0.,0.));
#10961=CARTESIAN_POINT('',(-0.143317017690053,0.,-1.23958209161204));
#10962=CARTESIAN_POINT('Origin',(-0.192154639568406,0.,-1.21321664662686));
#10963=CARTESIAN_POINT('',(-0.0523608139934479,0.,-1.24674050008925));
#10964=CARTESIAN_POINT('Origin',(0.,0.,0.));
#10965=CARTESIAN_POINT('',(0.0523608139934481,0.,-1.24674050008925));
#10966=CARTESIAN_POINT('Origin',(7.52141045863017E-17,0.,-1.22833954473516));
#10967=CARTESIAN_POINT('',(0.143317017690053,0.,-1.23958209161204));
#10968=CARTESIAN_POINT('Origin',(0.,0.,0.));
#10969=CARTESIAN_POINT('',(0.246749348660852,0.,-1.22320001975977));
#10970=CARTESIAN_POINT('Origin',(0.192154639568406,0.,-1.21321664662686));
#10971=CARTESIAN_POINT('',(0.335465908756113,0.,-1.20190105810224));
#10972=CARTESIAN_POINT('Origin',(0.,0.,0.));
#10973=CARTESIAN_POINT('',(0.435062095450087,0.,-1.16954029537568));
#10974=CARTESIAN_POINT('Origin',(0.379577794185951,0.,-1.1682203282434));
#10975=CARTESIAN_POINT('',(0.519354515801077,0.,-1.13462523166105));
#10976=CARTESIAN_POINT('Origin',(0.,0.,0.));
#10977=CARTESIAN_POINT('',(0.612662169561028,0.,-1.08708260743774));
#10978=CARTESIAN_POINT('Origin',(0.557654483764164,0.,-1.0944585482776));
#10979=CARTESIAN_POINT('',(0.690454891028201,0.,-1.0394111664111));
#10980=CARTESIAN_POINT('Origin',(0.,0.,0.));
#10981=CARTESIAN_POINT('',(0.775176467748211,0.,-0.977857337884349));
#10982=CARTESIAN_POINT('Origin',(0.721999869202979,0.,-0.993747566553533));
#10983=CARTESIAN_POINT('',(0.844553975349804,0.,-0.918603348636233));
#10984=CARTESIAN_POINT('Origin',(0.,0.,0.));
#10985=CARTESIAN_POINT('',(0.918603348636233,0.,-0.844553975349804));
#10986=CARTESIAN_POINT('Origin',(0.86856722168183,0.,-0.86856722168183));
#10987=CARTESIAN_POINT('',(0.977857337884349,0.,-0.775176467748211));
#10988=CARTESIAN_POINT('Origin',(0.,0.,0.));
#10989=CARTESIAN_POINT('',(1.0394111664111,0.,-0.690454891028201));
#10990=CARTESIAN_POINT('Origin',(0.993747566553533,0.,-0.721999869202979));
#10991=CARTESIAN_POINT('',(1.08708260743774,0.,-0.612662169561028));
#10992=CARTESIAN_POINT('Origin',(0.,0.,0.));
#10993=CARTESIAN_POINT('',(1.13462523166105,0.,-0.519354515801077));
#10994=CARTESIAN_POINT('Origin',(1.0944585482776,0.,-0.557654483764164));
#10995=CARTESIAN_POINT('',(1.16954029537568,0.,-0.43506209545009));
#10996=CARTESIAN_POINT('Origin',(0.,0.,0.));
#10997=CARTESIAN_POINT('',(1.20190105810224,0.,-0.33546590875611));
#10998=CARTESIAN_POINT('Origin',(1.1682203282434,0.,-0.379577794185951));
#10999=CARTESIAN_POINT('',(1.22320001975977,0.,-0.246749348660852));
#11000=CARTESIAN_POINT('Origin',(0.,0.,0.));
#11001=CARTESIAN_POINT('',(1.23958209161204,0.,-0.143317017690053));
#11002=CARTESIAN_POINT('Origin',(1.21321664662686,0.,-0.192154639568406));
#11003=CARTESIAN_POINT('',(1.24674050008925,0.,-0.052360813993451));
#11004=CARTESIAN_POINT('Origin',(0.,0.,0.));
#11005=CARTESIAN_POINT('',(1.24674050008925,0.,0.052360813993451));
#11006=CARTESIAN_POINT('Origin',(1.22833954473516,0.,0.));
#11007=CARTESIAN_POINT('Origin',(0.,0.,0.));
#11008=CARTESIAN_POINT('Origin',(0.,0.,0.));
#11009=CARTESIAN_POINT('',(-1.4,-0.1,1.71450551880629E-16));
#11010=CARTESIAN_POINT('Origin',(0.,-0.1,0.));
#11011=CARTESIAN_POINT('',(-1.4,0.,-1.71450551880629E-16));
#11012=CARTESIAN_POINT('Origin',(0.,-0.1,0.));
#11013=CARTESIAN_POINT('Origin',(0.,0.75,0.));
#11014=CARTESIAN_POINT('',(-1.4,0.75,1.71450551880629E-16));
#11015=CARTESIAN_POINT('Origin',(0.,0.75,0.));
#11016=CARTESIAN_POINT('',(1.22320001975977,0.75,0.246749348660852));
#11017=CARTESIAN_POINT('',(1.23958209161204,0.75,0.143317017690053));
#11018=CARTESIAN_POINT('Origin',(1.21321664662686,0.75,0.192154639568406));
#11019=CARTESIAN_POINT('',(1.24674050008925,0.75,0.052360813993448));
#11020=CARTESIAN_POINT('Origin',(0.,0.75,0.));
#11021=CARTESIAN_POINT('',(1.24674050008925,0.75,-0.052360813993448));
#11022=CARTESIAN_POINT('Origin',(1.22833954473516,0.75,0.));
#11023=CARTESIAN_POINT('',(1.23958209161204,0.75,-0.143317017690053));
#11024=CARTESIAN_POINT('Origin',(0.,0.75,0.));
#11025=CARTESIAN_POINT('',(1.22320001975977,0.75,-0.246749348660852));
#11026=CARTESIAN_POINT('Origin',(1.21321664662686,0.75,-0.192154639568406));
#11027=CARTESIAN_POINT('',(1.20190105810224,0.75,-0.335465908756113));
#11028=CARTESIAN_POINT('Origin',(0.,0.75,0.));
#11029=CARTESIAN_POINT('',(1.16954029537568,0.75,-0.435062095450087));
#11030=CARTESIAN_POINT('Origin',(1.1682203282434,0.75,-0.379577794185951));
#11031=CARTESIAN_POINT('',(1.13462523166105,0.75,-0.519354515801077));
#11032=CARTESIAN_POINT('Origin',(0.,0.75,0.));
#11033=CARTESIAN_POINT('',(1.08708260743774,0.75,-0.612662169561028));
#11034=CARTESIAN_POINT('Origin',(1.0944585482776,0.75,-0.557654483764164));
#11035=CARTESIAN_POINT('',(1.0394111664111,0.75,-0.690454891028201));
#11036=CARTESIAN_POINT('Origin',(0.,0.75,0.));
#11037=CARTESIAN_POINT('',(0.977857337884349,0.75,-0.775176467748211));
#11038=CARTESIAN_POINT('Origin',(0.993747566553533,0.75,-0.721999869202979));
#11039=CARTESIAN_POINT('',(0.918603348636233,0.75,-0.844553975349804));
#11040=CARTESIAN_POINT('Origin',(0.,0.75,0.));
#11041=CARTESIAN_POINT('',(0.844553975349804,0.75,-0.918603348636233));
#11042=CARTESIAN_POINT('Origin',(0.86856722168183,0.75,-0.86856722168183));
#11043=CARTESIAN_POINT('',(0.775176467748211,0.75,-0.977857337884349));
#11044=CARTESIAN_POINT('Origin',(0.,0.75,0.));
#11045=CARTESIAN_POINT('',(0.690454891028201,0.75,-1.0394111664111));
#11046=CARTESIAN_POINT('Origin',(0.721999869202979,0.75,-0.993747566553533));
#11047=CARTESIAN_POINT('',(0.612662169561028,0.75,-1.08708260743774));
#11048=CARTESIAN_POINT('Origin',(0.,0.75,0.));
#11049=CARTESIAN_POINT('',(0.519354515801077,0.75,-1.13462523166105));
#11050=CARTESIAN_POINT('Origin',(0.557654483764164,0.75,-1.0944585482776));
#11051=CARTESIAN_POINT('',(0.435062095450087,0.75,-1.16954029537568));
#11052=CARTESIAN_POINT('Origin',(0.,0.75,0.));
#11053=CARTESIAN_POINT('',(0.335465908756113,0.75,-1.20190105810224));
#11054=CARTESIAN_POINT('Origin',(0.379577794185951,0.75,-1.1682203282434));
#11055=CARTESIAN_POINT('',(0.246749348660852,0.75,-1.22320001975977));
#11056=CARTESIAN_POINT('Origin',(0.,0.75,0.));
#11057=CARTESIAN_POINT('',(0.143317017690053,0.75,-1.23958209161204));
#11058=CARTESIAN_POINT('Origin',(0.192154639568406,0.75,-1.21321664662686));
#11059=CARTESIAN_POINT('',(0.0523608139934481,0.75,-1.24674050008925));
#11060=CARTESIAN_POINT('Origin',(0.,0.75,0.));
#11061=CARTESIAN_POINT('',(-0.0523608139934479,0.75,-1.24674050008925));
#11062=CARTESIAN_POINT('Origin',(7.52141045863017E-17,0.75,-1.22833954473516));
#11063=CARTESIAN_POINT('',(-0.143317017690053,0.75,-1.23958209161204));
#11064=CARTESIAN_POINT('Origin',(0.,0.75,0.));
#11065=CARTESIAN_POINT('',(-0.246749348660852,0.75,-1.22320001975977));
#11066=CARTESIAN_POINT('Origin',(-0.192154639568406,0.75,-1.21321664662686));
#11067=CARTESIAN_POINT('',(-0.335465908756113,0.75,-1.20190105810224));
#11068=CARTESIAN_POINT('Origin',(0.,0.75,0.));
#11069=CARTESIAN_POINT('',(-0.435062095450087,0.75,-1.16954029537568));
#11070=CARTESIAN_POINT('Origin',(-0.379577794185951,0.75,-1.1682203282434));
#11071=CARTESIAN_POINT('',(-0.519354515801077,0.75,-1.13462523166105));
#11072=CARTESIAN_POINT('Origin',(0.,0.75,0.));
#11073=CARTESIAN_POINT('',(-0.612662169561028,0.75,-1.08708260743774));
#11074=CARTESIAN_POINT('Origin',(-0.557654483764164,0.75,-1.0944585482776));
#11075=CARTESIAN_POINT('',(-0.690454891028201,0.75,-1.0394111664111));
#11076=CARTESIAN_POINT('Origin',(0.,0.75,0.));
#11077=CARTESIAN_POINT('',(-0.775176467748211,0.75,-0.977857337884348));
#11078=CARTESIAN_POINT('Origin',(-0.721999869202979,0.75,-0.993747566553533));
#11079=CARTESIAN_POINT('',(-0.844553975349804,0.75,-0.918603348636233));
#11080=CARTESIAN_POINT('Origin',(0.,0.75,0.));
#11081=CARTESIAN_POINT('',(-0.918603348636233,0.75,-0.844553975349804));
#11082=CARTESIAN_POINT('Origin',(-0.86856722168183,0.75,-0.86856722168183));
#11083=CARTESIAN_POINT('',(-0.977857337884349,0.75,-0.775176467748211));
#11084=CARTESIAN_POINT('Origin',(0.,0.75,0.));
#11085=CARTESIAN_POINT('',(-1.0394111664111,0.75,-0.690454891028201));
#11086=CARTESIAN_POINT('Origin',(-0.993747566553533,0.75,-0.721999869202979));
#11087=CARTESIAN_POINT('',(-1.08708260743774,0.75,-0.612662169561029));
#11088=CARTESIAN_POINT('Origin',(0.,0.75,0.));
#11089=CARTESIAN_POINT('',(-1.13462523166105,0.75,-0.519354515801077));
#11090=CARTESIAN_POINT('Origin',(-1.0944585482776,0.75,-0.557654483764164));
#11091=CARTESIAN_POINT('',(-1.16954029537568,0.75,-0.435062095450087));
#11092=CARTESIAN_POINT('Origin',(0.,0.75,0.));
#11093=CARTESIAN_POINT('',(-1.20190105810224,0.75,-0.335465908756113));
#11094=CARTESIAN_POINT('Origin',(-1.1682203282434,0.75,-0.379577794185951));
#11095=CARTESIAN_POINT('',(-1.22320001975977,0.75,-0.246749348660852));
#11096=CARTESIAN_POINT('Origin',(0.,0.75,0.));
#11097=CARTESIAN_POINT('',(-1.23958209161204,0.75,-0.143317017690053));
#11098=CARTESIAN_POINT('Origin',(-1.21321664662686,0.75,-0.192154639568406));
#11099=CARTESIAN_POINT('',(-1.24674050008925,0.75,-0.0523608139934482));
#11100=CARTESIAN_POINT('Origin',(0.,0.75,0.));
#11101=CARTESIAN_POINT('',(-1.24674050008925,0.75,0.0523608139934479));
#11102=CARTESIAN_POINT('Origin',(-1.22833954473516,0.75,-1.50428209172603E-16));
#11103=CARTESIAN_POINT('',(-1.23958209161204,0.75,0.143317017690053));
#11104=CARTESIAN_POINT('Origin',(0.,0.75,0.));
#11105=CARTESIAN_POINT('',(-1.22320001975977,0.75,0.246749348660851));
#11106=CARTESIAN_POINT('Origin',(-1.21321664662686,0.75,0.192154639568406));
#11107=CARTESIAN_POINT('',(-1.20190105810224,0.75,0.335465908756113));
#11108=CARTESIAN_POINT('Origin',(0.,0.75,0.));
#11109=CARTESIAN_POINT('',(-1.16954029537568,0.75,0.435062095450087));
#11110=CARTESIAN_POINT('Origin',(-1.1682203282434,0.75,0.379577794185951));
#11111=CARTESIAN_POINT('',(-1.13462523166105,0.75,0.519354515801077));
#11112=CARTESIAN_POINT('Origin',(0.,0.75,0.));
#11113=CARTESIAN_POINT('',(-1.08708260743774,0.75,0.612662169561028));
#11114=CARTESIAN_POINT('Origin',(-1.0944585482776,0.75,0.557654483764164));
#11115=CARTESIAN_POINT('',(-1.0394111664111,0.75,0.690454891028201));
#11116=CARTESIAN_POINT('Origin',(0.,0.75,0.));
#11117=CARTESIAN_POINT('',(-0.977857337884348,0.75,0.775176467748211));
#11118=CARTESIAN_POINT('Origin',(-0.993747566553533,0.75,0.721999869202979));
#11119=CARTESIAN_POINT('',(-0.918603348636233,0.75,0.844553975349804));
#11120=CARTESIAN_POINT('Origin',(0.,0.75,0.));
#11121=CARTESIAN_POINT('',(-0.844553975349804,0.75,0.918603348636233));
#11122=CARTESIAN_POINT('Origin',(-0.86856722168183,0.75,0.86856722168183));
#11123=CARTESIAN_POINT('',(-0.775176467748211,0.75,0.977857337884349));
#11124=CARTESIAN_POINT('Origin',(0.,0.75,0.));
#11125=CARTESIAN_POINT('',(-0.690454891028201,0.75,1.0394111664111));
#11126=CARTESIAN_POINT('Origin',(-0.721999869202979,0.75,0.993747566553533));
#11127=CARTESIAN_POINT('',(-0.612662169561029,0.75,1.08708260743774));
#11128=CARTESIAN_POINT('Origin',(0.,0.75,0.));
#11129=CARTESIAN_POINT('',(-0.519354515801077,0.75,1.13462523166105));
#11130=CARTESIAN_POINT('Origin',(-0.557654483764164,0.75,1.0944585482776));
#11131=CARTESIAN_POINT('',(-0.435062095450087,0.75,1.16954029537568));
#11132=CARTESIAN_POINT('Origin',(0.,0.75,0.));
#11133=CARTESIAN_POINT('',(-0.335465908756113,0.75,1.20190105810224));
#11134=CARTESIAN_POINT('Origin',(-0.379577794185951,0.75,1.1682203282434));
#11135=CARTESIAN_POINT('',(-0.246749348660852,0.75,1.22320001975977));
#11136=CARTESIAN_POINT('Origin',(0.,0.75,0.));
#11137=CARTESIAN_POINT('',(-0.143317017690053,0.75,1.23958209161204));
#11138=CARTESIAN_POINT('Origin',(-0.192154639568406,0.75,1.21321664662686));
#11139=CARTESIAN_POINT('',(-0.0523608139934483,0.75,1.24674050008925));
#11140=CARTESIAN_POINT('Origin',(0.,0.75,0.));
#11141=CARTESIAN_POINT('',(0.0523608139934478,0.75,1.24674050008925));
#11142=CARTESIAN_POINT('Origin',(-2.25642313758905E-16,0.75,1.22833954473516));
#11143=CARTESIAN_POINT('',(0.143317017690053,0.75,1.23958209161204));
#11144=CARTESIAN_POINT('Origin',(0.,0.75,0.));
#11145=CARTESIAN_POINT('',(0.246749348660851,0.75,1.22320001975977));
#11146=CARTESIAN_POINT('Origin',(0.192154639568406,0.75,1.21321664662686));
#11147=CARTESIAN_POINT('',(0.335465908756113,0.75,1.20190105810224));
#11148=CARTESIAN_POINT('Origin',(0.,0.75,0.));
#11149=CARTESIAN_POINT('',(0.435062095450087,0.75,1.16954029537568));
#11150=CARTESIAN_POINT('Origin',(0.379577794185951,0.75,1.1682203282434));
#11151=CARTESIAN_POINT('',(0.519354515801077,0.75,1.13462523166105));
#11152=CARTESIAN_POINT('Origin',(0.,0.75,0.));
#11153=CARTESIAN_POINT('',(0.612662169561028,0.75,1.08708260743774));
#11154=CARTESIAN_POINT('Origin',(0.557654483764164,0.75,1.0944585482776));
#11155=CARTESIAN_POINT('',(0.690454891028201,0.75,1.0394111664111));
#11156=CARTESIAN_POINT('Origin',(0.,0.75,0.));
#11157=CARTESIAN_POINT('',(0.775176467748211,0.75,0.977857337884349));
#11158=CARTESIAN_POINT('Origin',(0.721999869202979,0.75,0.993747566553533));
#11159=CARTESIAN_POINT('',(0.844553975349804,0.75,0.918603348636233));
#11160=CARTESIAN_POINT('Origin',(0.,0.75,0.));
#11161=CARTESIAN_POINT('',(0.918603348636233,0.75,0.844553975349804));
#11162=CARTESIAN_POINT('Origin',(0.86856722168183,0.75,0.86856722168183));
#11163=CARTESIAN_POINT('',(0.977857337884349,0.75,0.775176467748211));
#11164=CARTESIAN_POINT('Origin',(0.,0.75,0.));
#11165=CARTESIAN_POINT('',(1.0394111664111,0.75,0.690454891028201));
#11166=CARTESIAN_POINT('Origin',(0.993747566553533,0.75,0.72199986920298));
#11167=CARTESIAN_POINT('',(1.08708260743774,0.75,0.612662169561029));
#11168=CARTESIAN_POINT('Origin',(0.,0.75,0.));
#11169=CARTESIAN_POINT('',(1.13462523166105,0.75,0.519354515801077));
#11170=CARTESIAN_POINT('Origin',(1.0944585482776,0.75,0.557654483764164));
#11171=CARTESIAN_POINT('',(1.16954029537568,0.75,0.435062095450087));
#11172=CARTESIAN_POINT('Origin',(0.,0.75,0.));
#11173=CARTESIAN_POINT('',(1.20190105810224,0.75,0.335465908756113));
#11174=CARTESIAN_POINT('Origin',(1.1682203282434,0.75,0.379577794185952));
#11175=CARTESIAN_POINT('Origin',(0.,0.75,0.));
#11176=CARTESIAN_POINT('Origin',(0.,0.75,0.));
#11177=CARTESIAN_POINT('',(-1.4,0.75,1.71450551880629E-16));
#11178=CARTESIAN_POINT('Origin',(1.21321664662686,0.,0.192154639568406));
#11179=CARTESIAN_POINT('',(1.23958209161204,0.,0.14331701769005));
#11180=CARTESIAN_POINT('',(1.22320001975977,0.,0.246749348660855));
#11181=CARTESIAN_POINT('Origin',(0.,0.,0.));
#11182=CARTESIAN_POINT('',(1.20190105810224,0.,0.33546590875611));
#11183=CARTESIAN_POINT('Origin',(1.1682203282434,0.,0.379577794185952));
#11184=CARTESIAN_POINT('',(1.16954029537568,0.,0.43506209545009));
#11185=CARTESIAN_POINT('Origin',(0.,0.,0.));
#11186=CARTESIAN_POINT('',(1.13462523166105,0.,0.519354515801074));
#11187=CARTESIAN_POINT('Origin',(1.0944585482776,0.,0.557654483764164));
#11188=CARTESIAN_POINT('',(1.08708260743774,0.,0.612662169561031));
#11189=CARTESIAN_POINT('Origin',(0.,0.,0.));
#11190=CARTESIAN_POINT('',(1.03941116641111,0.,0.690454891028199));
#11191=CARTESIAN_POINT('Origin',(0.993747566553533,0.,0.72199986920298));
#11192=CARTESIAN_POINT('',(0.977857337884347,0.,0.775176467748214));
#11193=CARTESIAN_POINT('Origin',(0.,0.,0.));
#11194=CARTESIAN_POINT('',(0.918603348636235,0.,0.844553975349802));
#11195=CARTESIAN_POINT('Origin',(0.86856722168183,0.,0.86856722168183));
#11196=CARTESIAN_POINT('',(0.844553975349802,0.,0.918603348636235));
#11197=CARTESIAN_POINT('Origin',(0.,0.,0.));
#11198=CARTESIAN_POINT('',(0.775176467748213,0.,0.977857337884347));
#11199=CARTESIAN_POINT('Origin',(0.721999869202979,0.,0.993747566553533));
#11200=CARTESIAN_POINT('',(0.690454891028198,0.,1.03941116641111));
#11201=CARTESIAN_POINT('Origin',(0.,0.,0.));
#11202=CARTESIAN_POINT('',(0.612662169561031,0.,1.08708260743774));
#11203=CARTESIAN_POINT('Origin',(0.557654483764164,0.,1.0944585482776));
#11204=CARTESIAN_POINT('',(0.519354515801074,0.,1.13462523166105));
#11205=CARTESIAN_POINT('Origin',(0.,0.,0.));
#11206=CARTESIAN_POINT('',(0.43506209545009,0.,1.16954029537568));
#11207=CARTESIAN_POINT('Origin',(0.379577794185951,0.,1.1682203282434));
#11208=CARTESIAN_POINT('',(0.33546590875611,0.,1.20190105810224));
#11209=CARTESIAN_POINT('Origin',(0.,0.,0.));
#11210=CARTESIAN_POINT('',(0.246749348660854,0.,1.22320001975977));
#11211=CARTESIAN_POINT('Origin',(0.192154639568406,0.,1.21321664662686));
#11212=CARTESIAN_POINT('',(0.14331701769005,0.,1.23958209161204));
#11213=CARTESIAN_POINT('Origin',(0.,0.,0.));
#11214=CARTESIAN_POINT('',(0.0523608139934508,0.,1.24674050008925));
#11215=CARTESIAN_POINT('Origin',(-2.25642313758905E-16,0.,1.22833954473516));
#11216=CARTESIAN_POINT('',(-0.0523608139934513,0.,1.24674050008925));
#11217=CARTESIAN_POINT('Origin',(0.,0.,0.));
#11218=CARTESIAN_POINT('',(-0.14331701769005,0.,1.23958209161204));
#11219=CARTESIAN_POINT('Origin',(-0.192154639568406,0.,1.21321664662686));
#11220=CARTESIAN_POINT('',(-0.246749348660855,0.,1.22320001975977));
#11221=CARTESIAN_POINT('Origin',(0.,0.,0.));
#11222=CARTESIAN_POINT('',(-0.33546590875611,0.,1.20190105810224));
#11223=CARTESIAN_POINT('Origin',(-0.379577794185951,0.,1.1682203282434));
#11224=CARTESIAN_POINT('',(-0.43506209545009,0.,1.16954029537568));
#11225=CARTESIAN_POINT('Origin',(0.,0.,0.));
#11226=CARTESIAN_POINT('',(-0.519354515801074,0.,1.13462523166105));
#11227=CARTESIAN_POINT('Origin',(-0.557654483764164,0.,1.0944585482776));
#11228=CARTESIAN_POINT('',(-0.612662169561031,0.,1.08708260743774));
#11229=CARTESIAN_POINT('Origin',(0.,0.,0.));
#11230=CARTESIAN_POINT('',(-0.690454891028199,0.,1.03941116641111));
#11231=CARTESIAN_POINT('Origin',(-0.721999869202979,0.,0.993747566553533));
#11232=CARTESIAN_POINT('',(-0.775176467748213,0.,0.977857337884347));
#11233=CARTESIAN_POINT('Origin',(0.,0.,0.));
#11234=CARTESIAN_POINT('',(-0.844553975349802,0.,0.918603348636235));
#11235=CARTESIAN_POINT('Origin',(-0.86856722168183,0.,0.86856722168183));
#11236=CARTESIAN_POINT('',(-0.918603348636235,0.,0.844553975349802));
#11237=CARTESIAN_POINT('Origin',(0.,0.,0.));
#11238=CARTESIAN_POINT('',(-0.977857337884347,0.,0.775176467748213));
#11239=CARTESIAN_POINT('Origin',(-0.993747566553533,0.,0.721999869202979));
#11240=CARTESIAN_POINT('',(-1.03941116641111,0.,0.690454891028198));
#11241=CARTESIAN_POINT('Origin',(0.,0.,0.));
#11242=CARTESIAN_POINT('',(-1.08708260743774,0.,0.612662169561031));
#11243=CARTESIAN_POINT('Origin',(-1.0944585482776,0.,0.557654483764164));
#11244=CARTESIAN_POINT('',(-1.13462523166105,0.,0.519354515801074));
#11245=CARTESIAN_POINT('Origin',(0.,0.,0.));
#11246=CARTESIAN_POINT('',(-1.16954029537568,0.,0.43506209545009));
#11247=CARTESIAN_POINT('Origin',(-1.1682203282434,0.,0.379577794185951));
#11248=CARTESIAN_POINT('',(-1.20190105810224,0.,0.33546590875611));
#11249=CARTESIAN_POINT('Origin',(0.,0.,0.));
#11250=CARTESIAN_POINT('',(-1.22320001975977,0.,0.246749348660854));
#11251=CARTESIAN_POINT('Origin',(-1.21321664662686,0.,0.192154639568406));
#11252=CARTESIAN_POINT('',(-1.23958209161204,0.,0.14331701769005));
#11253=CARTESIAN_POINT('Origin',(0.,0.,0.));
#11254=CARTESIAN_POINT('',(-1.24674050008925,0.,0.0523608139934509));
#11255=CARTESIAN_POINT('Origin',(-1.22833954473516,0.,-1.50428209172603E-16));
#11256=CARTESIAN_POINT('',(-1.24674050008925,0.,-0.0523608139934512));
#11257=CARTESIAN_POINT('Origin',(0.,0.,0.));
#11258=CARTESIAN_POINT('',(-1.23958209161204,0.,-0.14331701769005));
#11259=CARTESIAN_POINT('Origin',(-1.21321664662686,0.,-0.192154639568406));
#11260=CARTESIAN_POINT('',(-1.22320001975977,0.,-0.246749348660855));
#11261=CARTESIAN_POINT('Origin',(0.,0.,0.));
#11262=CARTESIAN_POINT('',(-1.20190105810224,0.,-0.33546590875611));
#11263=CARTESIAN_POINT('Origin',(-1.1682203282434,0.,-0.379577794185951));
#11264=CARTESIAN_POINT('',(-1.16954029537568,0.,-0.43506209545009));
#11265=CARTESIAN_POINT('Origin',(0.,0.,0.));
#11266=CARTESIAN_POINT('',(-1.13462523166105,0.,-0.519354515801074));
#11267=CARTESIAN_POINT('Origin',(-1.0944585482776,0.,-0.557654483764164));
#11268=CARTESIAN_POINT('',(-1.08708260743774,0.,-0.612662169561031));
#11269=CARTESIAN_POINT('Origin',(0.,0.,0.));
#11270=CARTESIAN_POINT('',(-1.03941116641111,0.,-0.690454891028199));
#11271=CARTESIAN_POINT('Origin',(-0.993747566553533,0.,-0.721999869202979));
#11272=CARTESIAN_POINT('',(-0.977857337884347,0.,-0.775176467748213));
#11273=CARTESIAN_POINT('Origin',(0.,0.,0.));
#11274=CARTESIAN_POINT('',(-0.918603348636235,0.,-0.844553975349802));
#11275=CARTESIAN_POINT('Origin',(-0.86856722168183,0.,-0.86856722168183));
#11276=CARTESIAN_POINT('',(-0.844553975349802,0.,-0.918603348636235));
#11277=CARTESIAN_POINT('Origin',(0.,0.,0.));
#11278=CARTESIAN_POINT('',(-0.775176467748213,0.,-0.977857337884347));
#11279=CARTESIAN_POINT('Origin',(-0.721999869202979,0.,-0.993747566553533));
#11280=CARTESIAN_POINT('',(-0.690454891028198,0.,-1.03941116641111));
#11281=CARTESIAN_POINT('Origin',(0.,0.,0.));
#11282=CARTESIAN_POINT('',(-0.612662169561031,0.,-1.08708260743774));
#11283=CARTESIAN_POINT('Origin',(-0.557654483764164,0.,-1.0944585482776));
#11284=CARTESIAN_POINT('',(-0.519354515801074,0.,-1.13462523166105));
#11285=CARTESIAN_POINT('Origin',(0.,0.,0.));
#11286=CARTESIAN_POINT('',(-0.43506209545009,0.,-1.16954029537568));
#11287=CARTESIAN_POINT('Origin',(-0.379577794185951,0.,-1.1682203282434));
#11288=CARTESIAN_POINT('',(-0.33546590875611,0.,-1.20190105810224));
#11289=CARTESIAN_POINT('Origin',(0.,0.,0.));
#11290=CARTESIAN_POINT('',(-0.246749348660854,0.,-1.22320001975977));
#11291=CARTESIAN_POINT('Origin',(-0.192154639568406,0.,-1.21321664662686));
#11292=CARTESIAN_POINT('',(-0.14331701769005,0.,-1.23958209161204));
#11293=CARTESIAN_POINT('Origin',(0.,0.,0.));
#11294=CARTESIAN_POINT('',(-0.052360813993451,0.,-1.24674050008925));
#11295=CARTESIAN_POINT('Origin',(7.52141045863017E-17,0.,-1.22833954473516));
#11296=CARTESIAN_POINT('',(0.0523608139934511,0.,-1.24674050008925));
#11297=CARTESIAN_POINT('Origin',(0.,0.,0.));
#11298=CARTESIAN_POINT('',(0.14331701769005,0.,-1.23958209161204));
#11299=CARTESIAN_POINT('Origin',(0.192154639568406,0.,-1.21321664662686));
#11300=CARTESIAN_POINT('',(0.246749348660855,0.,-1.22320001975977));
#11301=CARTESIAN_POINT('Origin',(0.,0.,0.));
#11302=CARTESIAN_POINT('',(0.33546590875611,0.,-1.20190105810224));
#11303=CARTESIAN_POINT('Origin',(0.379577794185951,0.,-1.1682203282434));
#11304=CARTESIAN_POINT('',(0.43506209545009,0.,-1.16954029537568));
#11305=CARTESIAN_POINT('Origin',(0.,0.,0.));
#11306=CARTESIAN_POINT('',(0.519354515801074,0.,-1.13462523166105));
#11307=CARTESIAN_POINT('Origin',(0.557654483764164,0.,-1.0944585482776));
#11308=CARTESIAN_POINT('',(0.612662169561031,0.,-1.08708260743774));
#11309=CARTESIAN_POINT('Origin',(0.,0.,0.));
#11310=CARTESIAN_POINT('',(0.690454891028198,0.,-1.03941116641111));
#11311=CARTESIAN_POINT('Origin',(0.721999869202979,0.,-0.993747566553533));
#11312=CARTESIAN_POINT('',(0.775176467748213,0.,-0.977857337884347));
#11313=CARTESIAN_POINT('Origin',(0.,0.,0.));
#11314=CARTESIAN_POINT('',(0.844553975349802,0.,-0.918603348636235));
#11315=CARTESIAN_POINT('Origin',(0.86856722168183,0.,-0.86856722168183));
#11316=CARTESIAN_POINT('',(0.918603348636235,0.,-0.844553975349802));
#11317=CARTESIAN_POINT('Origin',(0.,0.,0.));
#11318=CARTESIAN_POINT('',(0.977857337884347,0.,-0.775176467748213));
#11319=CARTESIAN_POINT('Origin',(0.993747566553533,0.,-0.721999869202979));
#11320=CARTESIAN_POINT('',(1.03941116641111,0.,-0.690454891028198));
#11321=CARTESIAN_POINT('Origin',(0.,0.,0.));
#11322=CARTESIAN_POINT('',(1.08708260743774,0.,-0.612662169561031));
#11323=CARTESIAN_POINT('Origin',(1.0944585482776,0.,-0.557654483764164));
#11324=CARTESIAN_POINT('',(1.13462523166105,0.,-0.519354515801074));
#11325=CARTESIAN_POINT('Origin',(0.,0.,0.));
#11326=CARTESIAN_POINT('',(1.16954029537568,0.,-0.43506209545009));
#11327=CARTESIAN_POINT('Origin',(1.1682203282434,0.,-0.379577794185951));
#11328=CARTESIAN_POINT('',(1.20190105810224,0.,-0.33546590875611));
#11329=CARTESIAN_POINT('Origin',(0.,0.,0.));
#11330=CARTESIAN_POINT('',(1.22320001975977,0.,-0.246749348660855));
#11331=CARTESIAN_POINT('Origin',(1.21321664662686,0.,-0.192154639568406));
#11332=CARTESIAN_POINT('',(1.23958209161204,0.,-0.14331701769005));
#11333=CARTESIAN_POINT('Origin',(0.,0.,0.));
#11334=CARTESIAN_POINT('',(1.24674050008925,0.,0.052360813993451));
#11335=CARTESIAN_POINT('Origin',(1.22833954473516,0.,0.));
#11336=CARTESIAN_POINT('',(1.24674050008925,0.,-0.052360813993451));
#11337=CARTESIAN_POINT('Origin',(0.,0.,0.));
#11338=CARTESIAN_POINT('',(0.,0.,0.));
#11339=CARTESIAN_POINT('Origin',(0.7,0.,0.25));
#11340=CARTESIAN_POINT('',(0.7,0.16,0.4));
#11341=CARTESIAN_POINT('',(0.7,0.2,0.36));
#11342=CARTESIAN_POINT('',(0.7,0.1675,0.3925));
#11343=CARTESIAN_POINT('',(0.7,-0.16,0.4));
#11344=CARTESIAN_POINT('',(0.7,0.,0.4));
#11345=CARTESIAN_POINT('',(0.7,-0.2,0.36));
#11346=CARTESIAN_POINT('',(0.7,-0.1675,0.3925));
#11347=CARTESIAN_POINT('',(0.7,-0.2,0.04));
#11348=CARTESIAN_POINT('',(0.7,-0.2,0.125));
#11349=CARTESIAN_POINT('',(0.7,-0.16,0.));
#11350=CARTESIAN_POINT('',(0.7,-0.1925,0.0325));
#11351=CARTESIAN_POINT('',(0.7,0.16,0.));
#11352=CARTESIAN_POINT('',(0.7,0.,0.));
#11353=CARTESIAN_POINT('',(0.7,0.2,0.04));
#11354=CARTESIAN_POINT('',(0.7,0.1925,0.0325));
#11355=CARTESIAN_POINT('',(0.7,0.2,0.125));
#11356=CARTESIAN_POINT('Origin',(-0.4,-0.18,0.02));
#11357=CARTESIAN_POINT('',(-0.7,-0.2,0.04));
#11358=CARTESIAN_POINT('',(-0.4,-0.2,0.04));
#11359=CARTESIAN_POINT('',(-0.7,-0.16,0.));
#11360=CARTESIAN_POINT('',(-0.7,-0.1925,0.0325));
#11361=CARTESIAN_POINT('',(-0.4,-0.16,0.));
#11362=CARTESIAN_POINT('Origin',(-0.8,-0.2,0.));
#11363=CARTESIAN_POINT('',(-0.7,-0.2,0.36));
#11364=CARTESIAN_POINT('',(-0.4,-0.2,0.36));
#11365=CARTESIAN_POINT('',(-0.7,-0.2,0.125));
#11366=CARTESIAN_POINT('Origin',(-0.4,-0.18,0.38));
#11367=CARTESIAN_POINT('',(-0.7,-0.16,0.4));
#11368=CARTESIAN_POINT('',(-0.4,-0.16,0.4));
#11369=CARTESIAN_POINT('',(-0.7,-0.1675,0.3925));
#11370=CARTESIAN_POINT('Origin',(0.,0.,0.4));
#11371=CARTESIAN_POINT('',(-0.7,0.16,0.4));
#11372=CARTESIAN_POINT('',(0.4,0.16,0.4));
#11373=CARTESIAN_POINT('',(-0.7,0.,0.4));
#11374=CARTESIAN_POINT('Origin',(-0.7,0.,0.25));
#11375=CARTESIAN_POINT('',(-0.7,0.2,0.36));
#11376=CARTESIAN_POINT('',(-0.7,0.1675,0.3925));
#11377=CARTESIAN_POINT('',(-0.7,0.2,0.04));
#11378=CARTESIAN_POINT('',(-0.7,0.2,0.125));
#11379=CARTESIAN_POINT('',(-0.7,0.16,0.));
#11380=CARTESIAN_POINT('',(-0.7,0.1925,0.0325));
#11381=CARTESIAN_POINT('',(-0.7,0.,0.));
#11382=CARTESIAN_POINT('Origin',(0.4,0.18,0.38));
#11383=CARTESIAN_POINT('',(0.4,0.2,0.36));
#11384=CARTESIAN_POINT('Origin',(0.8,0.2,0.));
#11385=CARTESIAN_POINT('',(0.4,0.2,0.04));
#11386=CARTESIAN_POINT('Origin',(0.4,0.18,0.02));
#11387=CARTESIAN_POINT('',(0.4,0.16,0.));
#11388=CARTESIAN_POINT('Origin',(0.,0.,0.));
#11389=CARTESIAN_POINT('',(0.,0.,0.));
#11390=CARTESIAN_POINT('Origin',(0.375,0.5,0.));
#11391=CARTESIAN_POINT('',(-0.375,0.5,-4.59242549680257E-17));
#11392=CARTESIAN_POINT('Origin',(0.,0.5,0.));
#11393=CARTESIAN_POINT('Origin',(0.,0.475,0.));
#11394=CARTESIAN_POINT('',(-0.425,0.45,-5.20474889637625E-17));
#11395=CARTESIAN_POINT('Origin',(0.,0.45,0.));
#11396=CARTESIAN_POINT('',(-0.4,0.475,-4.89858719658941E-17));
#11397=CARTESIAN_POINT('Origin',(0.,0.24,0.));
#11398=CARTESIAN_POINT('',(-0.425,0.0299999999999998,-5.20474889637625E-17));
#11399=CARTESIAN_POINT('Origin',(0.,0.0299999999999998,0.));
#11400=CARTESIAN_POINT('',(-0.425,0.24,-5.20474889637625E-17));
#11401=CARTESIAN_POINT('Origin',(0.,0.0150000000000001,0.));
#11402=CARTESIAN_POINT('',(-0.395,4.85722573273506E-17,-4.83735485663204E-17));
#11403=CARTESIAN_POINT('Origin',(0.,0.,0.));
#11404=CARTESIAN_POINT('',(-0.41,0.0150000000000001,-5.02105187650415E-17));
#11405=CARTESIAN_POINT('Origin',(0.27,0.,0.));
#11406=CARTESIAN_POINT('',(-0.27,0.,-3.30654635769785E-17));
#11407=CARTESIAN_POINT('Origin',(0.,0.,0.));
#11408=CARTESIAN_POINT('Origin',(0.,-0.02,0.));
#11409=CARTESIAN_POINT('',(-0.24505,-0.0498999999999999,3.00099698131059E-17));
#11410=CARTESIAN_POINT('Origin',(0.,-0.0498999999999999,0.));
#11411=CARTESIAN_POINT('',(-0.26,-0.02,-3.18408167778312E-17));
#11412=CARTESIAN_POINT('Origin',(0.,-0.995,0.));
#11413=CARTESIAN_POINT('',(-0.24505,-1.95495,3.00099698131059E-17));
#11414=CARTESIAN_POINT('Origin',(0.,-1.95495,0.));
#11415=CARTESIAN_POINT('',(-0.24505,-0.995,-3.00099698131059E-17));
#11416=CARTESIAN_POINT('Origin',(0.,-1.975,0.));
#11417=CARTESIAN_POINT('',(-0.2,-2.,-2.44929359829471E-17));
#11418=CARTESIAN_POINT('Origin',(0.,-2.,0.));
#11419=CARTESIAN_POINT('',(-0.225,-1.975,-2.75545529808154E-17));
#11420=CARTESIAN_POINT('Origin',(0.,-2.,0.));
#11421=CARTESIAN_POINT('Origin',(0.115470053837925,-0.5,-0.2));
#11422=CARTESIAN_POINT('',(0.23094010767585,-0.5,0.));
#11423=CARTESIAN_POINT('',(0.115470053837925,-0.5,-0.2));
#11424=CARTESIAN_POINT('',(0.23094010767585,-0.5,0.));
#11425=CARTESIAN_POINT('',(0.115470053837925,-0.8,-0.2));
#11426=CARTESIAN_POINT('',(0.115470053837925,-0.5,-0.2));
#11427=CARTESIAN_POINT('',(0.23094010767585,-0.8,0.));
#11428=CARTESIAN_POINT('',(0.23094010767585,-0.8,0.));
#11429=CARTESIAN_POINT('',(0.23094010767585,-0.5,0.));
#11430=CARTESIAN_POINT('Origin',(-0.115470053837925,-0.5,-0.2));
#11431=CARTESIAN_POINT('',(-0.115470053837925,-0.5,-0.2));
#11432=CARTESIAN_POINT('',(0.115470053837925,-0.5,-0.2));
#11433=CARTESIAN_POINT('',(-0.115470053837925,-0.8,-0.2));
#11434=CARTESIAN_POINT('',(-0.115470053837925,-0.5,-0.2));
#11435=CARTESIAN_POINT('',(0.115470053837925,-0.8,-0.2));
#11436=CARTESIAN_POINT('Origin',(-0.23094010767585,-0.5,-2.77555756156289E-17));
#11437=CARTESIAN_POINT('',(-0.23094010767585,-0.5,-2.82820063659975E-17));
#11438=CARTESIAN_POINT('',(-0.115470053837925,-0.5,-0.2));
#11439=CARTESIAN_POINT('',(-0.23094010767585,-0.8,-2.77555756156289E-17));
#11440=CARTESIAN_POINT('',(-0.23094010767585,-0.5,-2.82820063659975E-17));
#11441=CARTESIAN_POINT('',(-0.115470053837925,-0.8,-0.2));
#11442=CARTESIAN_POINT('Origin',(-0.115470053837925,-0.5,0.2));
#11443=CARTESIAN_POINT('',(-0.115470053837925,-0.5,0.2));
#11444=CARTESIAN_POINT('',(-0.23094010767585,-0.5,-2.82820063659975E-17));
#11445=CARTESIAN_POINT('',(-0.115470053837925,-0.8,0.2));
#11446=CARTESIAN_POINT('',(-0.115470053837925,-0.5,0.2));
#11447=CARTESIAN_POINT('',(-0.23094010767585,-0.8,-2.82820063659975E-17));
#11448=CARTESIAN_POINT('Origin',(0.115470053837925,-0.5,0.2));
#11449=CARTESIAN_POINT('',(0.115470053837925,-0.5,0.2));
#11450=CARTESIAN_POINT('',(-0.115470053837925,-0.5,0.2));
#11451=CARTESIAN_POINT('',(0.115470053837925,-0.8,0.2));
#11452=CARTESIAN_POINT('',(0.115470053837925,-0.5,0.2));
#11453=CARTESIAN_POINT('',(-0.115470053837925,-0.8,0.2));
#11454=CARTESIAN_POINT('Origin',(0.23094010767585,-0.5,0.));
#11455=CARTESIAN_POINT('',(0.115470053837925,-0.5,0.2));
#11456=CARTESIAN_POINT('',(0.115470053837925,-0.8,0.2));
#11457=CARTESIAN_POINT('Origin',(0.,-0.5,0.));
#11458=CARTESIAN_POINT('Origin',(0.,-0.8,0.));
#11459=CARTESIAN_POINT('',(0.,0.,0.));
#11460=CARTESIAN_POINT('Origin',(0.0721687836487032,0.,-0.125));
#11461=CARTESIAN_POINT('',(0.0721687836487032,0.,-0.125));
#11462=CARTESIAN_POINT('',(0.144337567297406,0.,0.));
#11463=CARTESIAN_POINT('',(0.117710979560879,0.,-0.0461186027918559));
#11464=CARTESIAN_POINT('',(0.0721687836487032,-0.25,-0.125));
#11465=CARTESIAN_POINT('',(0.0721687836487032,0.,-0.125));
#11466=CARTESIAN_POINT('',(0.144337567297406,-0.25,0.));
#11467=CARTESIAN_POINT('',(0.144337567297406,-0.25,0.));
#11468=CARTESIAN_POINT('',(0.144337567297406,0.,0.));
#11469=CARTESIAN_POINT('Origin',(-0.0721687836487032,0.,-0.125));
#11470=CARTESIAN_POINT('',(-0.0721687836487032,0.,-0.125));
#11471=CARTESIAN_POINT('',(0.0739156081756484,0.,-0.125));
#11472=CARTESIAN_POINT('',(-0.0721687836487032,-0.25,-0.125));
#11473=CARTESIAN_POINT('',(-0.0721687836487032,0.,-0.125));
#11474=CARTESIAN_POINT('',(0.0721687836487032,-0.25,-0.125));
#11475=CARTESIAN_POINT('Origin',(-0.144337567297406,0.,-4.16333634234434E-17));
#11476=CARTESIAN_POINT('',(-0.144337567297406,0.,-1.76762539787485E-17));
#11477=CARTESIAN_POINT('',(-0.0987953713852306,0.,-0.0788813972081442));
#11478=CARTESIAN_POINT('',(-0.144337567297406,-0.25,-2.77555756156289E-17));
#11479=CARTESIAN_POINT('',(-0.144337567297406,0.,-1.76762539787485E-17));
#11480=CARTESIAN_POINT('',(-0.0721687836487032,-0.25,-0.125));
#11481=CARTESIAN_POINT('Origin',(-0.0721687836487033,0.,0.125));
#11482=CARTESIAN_POINT('',(-0.0721687836487033,0.,0.125));
#11483=CARTESIAN_POINT('',(-0.0627109795608791,0.,0.141381397208144));
#11484=CARTESIAN_POINT('',(-0.0721687836487033,-0.25,0.125));
#11485=CARTESIAN_POINT('',(-0.0721687836487033,0.,0.125));
#11486=CARTESIAN_POINT('',(-0.144337567297406,-0.25,-1.76762539787485E-17));
#11487=CARTESIAN_POINT('Origin',(0.0721687836487032,0.,0.125));
#11488=CARTESIAN_POINT('',(0.0721687836487032,0.,0.125));
#11489=CARTESIAN_POINT('',(0.146084391824352,0.,0.125));
#11490=CARTESIAN_POINT('',(0.0721687836487032,-0.25,0.125));
#11491=CARTESIAN_POINT('',(0.0721687836487032,0.,0.125));
#11492=CARTESIAN_POINT('',(-0.0721687836487033,-0.25,0.125));
#11493=CARTESIAN_POINT('Origin',(0.144337567297406,0.,0.));
#11494=CARTESIAN_POINT('',(0.153795371385231,0.,-0.0163813972081441));
#11495=CARTESIAN_POINT('',(0.0721687836487032,-0.25,0.125));
#11496=CARTESIAN_POINT('Origin',(0.,-0.25,0.));
#11497=CARTESIAN_POINT('Origin',(0.22,0.,0.));
#11498=CARTESIAN_POINT('',(-0.22,-8.67361737988404E-18,-2.69422295812418E-17));
#11499=CARTESIAN_POINT('Origin',(0.,0.,0.));
#11500=CARTESIAN_POINT('Origin',(0.,-0.015,0.));
#11501=CARTESIAN_POINT('',(-0.24505,-0.02505,-3.00099698131059E-17));
#11502=CARTESIAN_POINT('Origin',(0.,-0.02505,0.));
#11503=CARTESIAN_POINT('',(-0.235,-0.015,-2.87791997799628E-17));
#11504=CARTESIAN_POINT('Origin',(0.,-0.3775,0.));
#11505=CARTESIAN_POINT('',(-0.24505,-0.72995,3.00099698131059E-17));
#11506=CARTESIAN_POINT('Origin',(0.,-0.72995,0.));
#11507=CARTESIAN_POINT('',(-0.24505,-0.3775,-3.00099698131059E-17));
#11508=CARTESIAN_POINT('Origin',(0.,-0.7625,0.));
#11509=CARTESIAN_POINT('',(-0.175,-0.8,-2.14313189850787E-17));
#11510=CARTESIAN_POINT('Origin',(0.,-0.8,0.));
#11511=CARTESIAN_POINT('',(-0.2125,-0.7625,-2.60237444818813E-17));
#11512=CARTESIAN_POINT('Origin',(0.,-0.8,0.));
#11513=CARTESIAN_POINT('',(0.,0.,0.));
#11514=CARTESIAN_POINT('Origin',(-1.,0.,0.35));
#11515=CARTESIAN_POINT('',(-1.,-0.26,0.6));
#11516=CARTESIAN_POINT('',(-1.,-0.3,0.56));
#11517=CARTESIAN_POINT('',(-1.,-0.2675,0.5925));
#11518=CARTESIAN_POINT('',(-1.,0.26,0.6));
#11519=CARTESIAN_POINT('',(-1.,0.,0.6));
#11520=CARTESIAN_POINT('',(-1.,0.3,0.56));
#11521=CARTESIAN_POINT('',(-1.,0.2675,0.5925));
#11522=CARTESIAN_POINT('',(-1.,0.3,0.04));
#11523=CARTESIAN_POINT('',(-1.,0.3,0.175));
#11524=CARTESIAN_POINT('',(-1.,0.26,0.));
#11525=CARTESIAN_POINT('',(-1.,0.2925,0.0325));
#11526=CARTESIAN_POINT('',(-1.,-0.26,0.));
#11527=CARTESIAN_POINT('',(-1.,0.,0.));
#11528=CARTESIAN_POINT('',(-1.,-0.3,0.04));
#11529=CARTESIAN_POINT('',(-1.,-0.2925,0.0325));
#11530=CARTESIAN_POINT('',(-1.,-0.3,0.175));
#11531=CARTESIAN_POINT('Origin',(0.75,0.28,0.02));
#11532=CARTESIAN_POINT('',(1.,0.3,0.04));
#11533=CARTESIAN_POINT('',(0.75,0.3,0.04));
#11534=CARTESIAN_POINT('',(1.,0.26,0.));
#11535=CARTESIAN_POINT('',(1.,0.2925,0.0325));
#11536=CARTESIAN_POINT('',(0.75,0.26,0.));
#11537=CARTESIAN_POINT('Origin',(1.5,0.3,0.));
#11538=CARTESIAN_POINT('',(1.,0.3,0.56));
#11539=CARTESIAN_POINT('',(0.75,0.3,0.56));
#11540=CARTESIAN_POINT('',(1.,0.3,0.175));
#11541=CARTESIAN_POINT('Origin',(0.75,0.28,0.58));
#11542=CARTESIAN_POINT('',(1.,0.26,0.6));
#11543=CARTESIAN_POINT('',(0.75,0.26,0.6));
#11544=CARTESIAN_POINT('',(1.,0.2675,0.5925));
#11545=CARTESIAN_POINT('Origin',(0.,0.,0.6));
#11546=CARTESIAN_POINT('',(1.,-0.26,0.6));
#11547=CARTESIAN_POINT('',(-0.75,-0.26,0.6));
#11548=CARTESIAN_POINT('',(1.,0.,0.6));
#11549=CARTESIAN_POINT('Origin',(1.,0.,0.35));
#11550=CARTESIAN_POINT('',(1.,-0.26,0.));
#11551=CARTESIAN_POINT('',(1.,-0.3,0.04));
#11552=CARTESIAN_POINT('',(1.,-0.2925,0.0325));
#11553=CARTESIAN_POINT('',(1.,0.,0.));
#11554=CARTESIAN_POINT('',(1.,-0.3,0.56));
#11555=CARTESIAN_POINT('',(1.,-0.2675,0.5925));
#11556=CARTESIAN_POINT('',(1.,-0.3,0.175));
#11557=CARTESIAN_POINT('Origin',(0.,0.,0.));
#11558=CARTESIAN_POINT('',(-0.75,-0.26,0.));
#11559=CARTESIAN_POINT('Origin',(-0.75,-0.28,0.58));
#11560=CARTESIAN_POINT('',(-0.75,-0.3,0.56));
#11561=CARTESIAN_POINT('Origin',(-0.75,-0.28,0.02));
#11562=CARTESIAN_POINT('',(-0.75,-0.3,0.04));
#11563=CARTESIAN_POINT('Origin',(-1.5,-0.3,0.));
#11564=CARTESIAN_POINT('',(0.,0.,0.));
#11565=CARTESIAN_POINT('Origin',(0.,0.,0.));
#11566=CARTESIAN_POINT('',(-0.42,0.16,5.14351655641888E-17));
#11567=CARTESIAN_POINT('Origin',(0.,0.16,0.));
#11568=CARTESIAN_POINT('',(-0.42,0.,5.14351655641888E-17));
#11569=CARTESIAN_POINT('',(-0.42,0.,5.14351655641888E-17));
#11570=CARTESIAN_POINT('Origin',(0.,0.,0.));
#11571=CARTESIAN_POINT('Origin',(0.,0.,0.));
#11572=CARTESIAN_POINT('',(-0.8,0.16,9.79717439317883E-17));
#11573=CARTESIAN_POINT('Origin',(0.,0.16,0.));
#11574=CARTESIAN_POINT('',(-0.8,0.,9.79717439317883E-17));
#11575=CARTESIAN_POINT('',(-0.8,0.,9.79717439317883E-17));
#11576=CARTESIAN_POINT('Origin',(0.,0.,0.));
#11577=CARTESIAN_POINT('Origin',(0.,0.16,0.));
#11578=CARTESIAN_POINT('Origin',(0.,0.,0.));
#11579=CARTESIAN_POINT('',(0.,0.,0.));
#11580=CARTESIAN_POINT('Origin',(0.,0.067277284513851,0.));
#11581=CARTESIAN_POINT('',(-0.375277674973257,0.0768195421087395,0.65));
#11582=CARTESIAN_POINT('',(0.375277674973257,0.0768195421087395,0.65));
#11583=CARTESIAN_POINT('Ctrl Pts',(-0.375277674973257,0.0768195421087395,
0.65));
#11584=CARTESIAN_POINT('Ctrl Pts',(1.66533453693773E-13,-0.0315137912242439,
0.65));
#11585=CARTESIAN_POINT('Ctrl Pts',(0.375277674973257,0.0768195421087394,
0.65));
#11586=CARTESIAN_POINT('',(-0.750555349946514,0.0768195421087394,-9.19165206894919E-17));
#11587=CARTESIAN_POINT('Ctrl Pts',(-0.750555349946514,0.0768195421087394,
-9.19165206894919E-17));
#11588=CARTESIAN_POINT('Ctrl Pts',(-0.562916512459802,-0.0315137912242434,
0.325000000000144));
#11589=CARTESIAN_POINT('Ctrl Pts',(-0.375277674973257,0.0768195421087395,
0.65));
#11590=CARTESIAN_POINT('',(-0.6175,-2.77555756156289E-17,-7.5621939847349E-17));
#11591=CARTESIAN_POINT('',(-0.734027674973257,0.067277284513851,-8.98924642641573E-17));
#11592=CARTESIAN_POINT('Origin',(0.,0.,0.));
#11593=CARTESIAN_POINT('',(-0.375277674973257,0.0768195421087395,-0.65));
#11594=CARTESIAN_POINT('Ctrl Pts',(-0.375277674973257,0.0768195421087395,
-0.65));
#11595=CARTESIAN_POINT('Ctrl Pts',(-0.562916512459968,-0.0315137912242437,
-0.324999999999856));
#11596=CARTESIAN_POINT('Ctrl Pts',(-0.750555349946514,0.0768195421087395,
-9.19165206894919E-17));
#11597=CARTESIAN_POINT('',(0.375277674973257,0.0768195421087395,-0.65));
#11598=CARTESIAN_POINT('Ctrl Pts',(0.375277674973257,0.0768195421087395,
-0.65));
#11599=CARTESIAN_POINT('Ctrl Pts',(-1.66144875635155E-13,-0.0315137912242437,
-0.65));
#11600=CARTESIAN_POINT('Ctrl Pts',(-0.375277674973257,0.0768195421087395,
-0.65));
#11601=CARTESIAN_POINT('',(0.750555349946514,0.0768195421087394,0.));
#11602=CARTESIAN_POINT('Ctrl Pts',(0.750555349946514,0.0768195421087394,
0.));
#11603=CARTESIAN_POINT('Ctrl Pts',(0.562916512459802,-0.0315137912242436,
-0.325000000000144));
#11604=CARTESIAN_POINT('Ctrl Pts',(0.375277674973257,0.0768195421087395,
-0.65));
#11605=CARTESIAN_POINT('Ctrl Pts',(0.375277674973257,0.0768195421087394,
0.65));
#11606=CARTESIAN_POINT('Ctrl Pts',(0.562916512459968,-0.0315137912242439,
0.324999999999856));
#11607=CARTESIAN_POINT('Ctrl Pts',(0.750555349946514,0.0768195421087394,
0.));
#11608=CARTESIAN_POINT('Origin',(0.,0.612722715486149,0.));
#11609=CARTESIAN_POINT('',(-0.6175,0.68,-7.5621939847349E-17));
#11610=CARTESIAN_POINT('Origin',(0.,0.68,0.));
#11611=CARTESIAN_POINT('',(-0.750555349946514,0.603180457891261,-9.19165206894919E-17));
#11612=CARTESIAN_POINT('',(-0.734027674973257,0.612722715486149,-8.98924642641573E-17));
#11613=CARTESIAN_POINT('',(-0.375277674973257,0.603180457891261,0.65));
#11614=CARTESIAN_POINT('Ctrl Pts',(-0.375277674973257,0.603180457891261,
0.65));
#11615=CARTESIAN_POINT('Ctrl Pts',(-0.562916512459968,0.711513791224243,
0.324999999999856));
#11616=CARTESIAN_POINT('Ctrl Pts',(-0.750555349946514,0.603180457891261,
-9.19165206894919E-17));
#11617=CARTESIAN_POINT('',(0.375277674973257,0.603180457891261,0.65));
#11618=CARTESIAN_POINT('Ctrl Pts',(0.375277674973257,0.603180457891261,
0.65));
#11619=CARTESIAN_POINT('Ctrl Pts',(-1.66755498298699E-13,0.711513791224244,
0.65));
#11620=CARTESIAN_POINT('Ctrl Pts',(-0.375277674973257,0.603180457891261,
0.65));
#11621=CARTESIAN_POINT('',(0.750555349946514,0.603180457891261,0.));
#11622=CARTESIAN_POINT('Ctrl Pts',(0.750555349946514,0.603180457891261,
0.));
#11623=CARTESIAN_POINT('Ctrl Pts',(0.562916512459802,0.711513791224244,
0.325000000000144));
#11624=CARTESIAN_POINT('Ctrl Pts',(0.375277674973257,0.603180457891261,
0.65));
#11625=CARTESIAN_POINT('',(0.375277674973257,0.603180457891261,-0.65));
#11626=CARTESIAN_POINT('Ctrl Pts',(0.375277674973257,0.603180457891261,
-0.65));
#11627=CARTESIAN_POINT('Ctrl Pts',(0.562916512459969,0.711513791224244,
-0.324999999999856));
#11628=CARTESIAN_POINT('Ctrl Pts',(0.750555349946514,0.603180457891261,
0.));
#11629=CARTESIAN_POINT('',(-0.375277674973257,0.603180457891261,-0.65));
#11630=CARTESIAN_POINT('Ctrl Pts',(-0.375277674973257,0.603180457891261,
-0.65));
#11631=CARTESIAN_POINT('Ctrl Pts',(1.66422431391311E-13,0.711513791224244,
-0.65));
#11632=CARTESIAN_POINT('Ctrl Pts',(0.375277674973257,0.603180457891261,
-0.65));
#11633=CARTESIAN_POINT('Ctrl Pts',(-0.750555349946514,0.603180457891261,
-9.19165206894919E-17));
#11634=CARTESIAN_POINT('Ctrl Pts',(-0.562916512459802,0.711513791224244,
-0.325000000000144));
#11635=CARTESIAN_POINT('Ctrl Pts',(-0.375277674973257,0.603180457891261,
-0.65));
#11636=CARTESIAN_POINT('Origin',(0.375277674973257,0.,-0.65));
#11637=CARTESIAN_POINT('',(-0.375277674973257,0.,-0.65));
#11638=CARTESIAN_POINT('',(0.375277674973257,0.,-0.65));
#11639=CARTESIAN_POINT('Origin',(-0.375277674973257,0.,-0.65));
#11640=CARTESIAN_POINT('',(-0.750555349946514,0.,-9.19165206894919E-17));
#11641=CARTESIAN_POINT('Origin',(-0.750555349946514,0.,-9.19165206894919E-17));
#11642=CARTESIAN_POINT('',(-0.375277674973257,0.,0.65));
#11643=CARTESIAN_POINT('Origin',(0.,0.,0.));
#11644=CARTESIAN_POINT('',(-0.338975,0.68,4.15124648740974E-17));
#11645=CARTESIAN_POINT('Origin',(0.,0.68,0.));
#11646=CARTESIAN_POINT('',(-0.338975,0.,4.15124648740974E-17));
#11647=CARTESIAN_POINT('',(-0.338975,0.,4.15124648740974E-17));
#11648=CARTESIAN_POINT('Origin',(0.,0.,0.));
#11649=CARTESIAN_POINT('Origin',(-0.375277674973257,0.,0.65));
#11650=CARTESIAN_POINT('',(0.375277674973257,0.,0.65));
#11651=CARTESIAN_POINT('Origin',(0.750555349946514,0.,0.));
#11652=CARTESIAN_POINT('',(0.750555349946514,0.,0.));
#11653=CARTESIAN_POINT('Origin',(0.375277674973257,0.,0.65));
#11654=CARTESIAN_POINT('Origin',(0.,0.68,-1.11022302462516E-16));
#11655=CARTESIAN_POINT('Origin',(0.,0.,-1.11022302462516E-16));
#11656=CARTESIAN_POINT('',(0.,0.,0.));
#11657=CARTESIAN_POINT('',(0.,0.,0.));
#11658=CARTESIAN_POINT('',(0.,0.,0.));
#11659=CARTESIAN_POINT('',(0.,0.,0.));
#11660=CARTESIAN_POINT('',(0.,0.,0.));
#11661=CARTESIAN_POINT('',(0.,0.,0.));
#11662=CARTESIAN_POINT('',(0.,0.,0.));
#11663=CARTESIAN_POINT('',(0.,0.,0.));
#11664=CARTESIAN_POINT('',(-5.,-2.5,2.2));
#11665=CARTESIAN_POINT('',(5.,-2.5,2.2));
#11666=CARTESIAN_POINT('',(0.,0.,8.));
#11667=CARTESIAN_POINT('',(-3.2,0.5,4.8));
#11668=CARTESIAN_POINT('',(-3.2,0.66,4.8));
#11669=CARTESIAN_POINT('',(-3.2,-1.46,4.8));
#11670=CARTESIAN_POINT('',(-3.2,-2.14,4.8));
#11671=CARTESIAN_POINT('',(-3.2,0.5,11.2));
#11672=CARTESIAN_POINT('',(-3.2,0.66,11.2));
#11673=CARTESIAN_POINT('',(-3.2,-1.46,11.2));
#11674=CARTESIAN_POINT('',(-3.2,-2.14,11.2));
#11675=CARTESIAN_POINT('',(3.2,0.5,4.8));
#11676=CARTESIAN_POINT('',(3.2,0.66,4.8));
#11677=CARTESIAN_POINT('',(3.2,-1.46,4.8));
#11678=CARTESIAN_POINT('',(3.2,-2.14,4.8));
#11679=CARTESIAN_POINT('',(3.2,0.5,11.2));
#11680=CARTESIAN_POINT('',(3.2,0.66,11.2));
#11681=CARTESIAN_POINT('',(3.2,-1.46,11.2));
#11682=CARTESIAN_POINT('',(3.2,-2.14,11.2));
#11683=CARTESIAN_POINT('',(0.,0.,0.));
#11684=CARTESIAN_POINT('',(0.,0.,0.));
#11685=CARTESIAN_POINT('',(0.,0.,0.));
#11686=CARTESIAN_POINT('',(0.,0.,0.));
#11687=CARTESIAN_POINT('',(0.,0.,0.));
#11688=CARTESIAN_POINT('',(0.,0.,0.));
#11689=CARTESIAN_POINT('',(0.,0.,0.));
#11690=CARTESIAN_POINT('',(0.,0.,0.));
#11691=CARTESIAN_POINT('',(0.,-5.8,8.));
#11692=CARTESIAN_POINT('',(0.,-5.825,7.65));
#11693=CARTESIAN_POINT('',(0.,-7.2,8.));
#11694=CARTESIAN_POINT('',(0.,-1.25,9.8));
#11695=CARTESIAN_POINT('',(0.,2.85,9.8));
#11696=CARTESIAN_POINT('',(0.,5.,7.35));
#11697=CARTESIAN_POINT('',(0.,6.7,8.));
#11698=CARTESIAN_POINT('',(0.,6.86,8.));
#11699=CARTESIAN_POINT('',(0.,0.,0.));
#11700=CARTESIAN_POINT('',(0.,0.,0.));
#11701=UNCERTAINTY_MEASURE_WITH_UNIT(LENGTH_MEASURE(0.001),#11765,
'DISTANCE_ACCURACY_VALUE',
'Maximum model space distance between geometric entities at asserted c
onnectivities');
#11702=UNCERTAINTY_MEASURE_WITH_UNIT(LENGTH_MEASURE(0.001),#11765,
'DISTANCE_ACCURACY_VALUE',
'Maximum model space distance between geometric entities at asserted c
onnectivities');
#11703=UNCERTAINTY_MEASURE_WITH_UNIT(LENGTH_MEASURE(0.001),#11765,
'DISTANCE_ACCURACY_VALUE',
'Maximum model space distance between geometric entities at asserted c
onnectivities');
#11704=UNCERTAINTY_MEASURE_WITH_UNIT(LENGTH_MEASURE(0.001),#11765,
'DISTANCE_ACCURACY_VALUE',
'Maximum model space distance between geometric entities at asserted c
onnectivities');
#11705=UNCERTAINTY_MEASURE_WITH_UNIT(LENGTH_MEASURE(0.001),#11765,
'DISTANCE_ACCURACY_VALUE',
'Maximum model space distance between geometric entities at asserted c
onnectivities');
#11706=UNCERTAINTY_MEASURE_WITH_UNIT(LENGTH_MEASURE(0.001),#11765,
'DISTANCE_ACCURACY_VALUE',
'Maximum model space distance between geometric entities at asserted c
onnectivities');
#11707=UNCERTAINTY_MEASURE_WITH_UNIT(LENGTH_MEASURE(0.001),#11765,
'DISTANCE_ACCURACY_VALUE',
'Maximum model space distance between geometric entities at asserted c
onnectivities');
#11708=UNCERTAINTY_MEASURE_WITH_UNIT(LENGTH_MEASURE(0.001),#11765,
'DISTANCE_ACCURACY_VALUE',
'Maximum model space distance between geometric entities at asserted c
onnectivities');
#11709=UNCERTAINTY_MEASURE_WITH_UNIT(LENGTH_MEASURE(0.001),#11765,
'DISTANCE_ACCURACY_VALUE',
'Maximum model space distance between geometric entities at asserted c
onnectivities');
#11710=UNCERTAINTY_MEASURE_WITH_UNIT(LENGTH_MEASURE(0.001),#11765,
'DISTANCE_ACCURACY_VALUE',
'Maximum model space distance between geometric entities at asserted c
onnectivities');
#11711=UNCERTAINTY_MEASURE_WITH_UNIT(LENGTH_MEASURE(0.001),#11765,
'DISTANCE_ACCURACY_VALUE',
'Maximum model space distance between geometric entities at asserted c
onnectivities');
#11712=UNCERTAINTY_MEASURE_WITH_UNIT(LENGTH_MEASURE(0.001),#11765,
'DISTANCE_ACCURACY_VALUE',
'Maximum model space distance between geometric entities at asserted c
onnectivities');
#11713=UNCERTAINTY_MEASURE_WITH_UNIT(LENGTH_MEASURE(0.001),#11765,
'DISTANCE_ACCURACY_VALUE',
'Maximum model space distance between geometric entities at asserted c
onnectivities');
#11714=UNCERTAINTY_MEASURE_WITH_UNIT(LENGTH_MEASURE(0.001),#11765,
'DISTANCE_ACCURACY_VALUE',
'Maximum model space distance between geometric entities at asserted c
onnectivities');
#11715=UNCERTAINTY_MEASURE_WITH_UNIT(LENGTH_MEASURE(0.001),#11765,
'DISTANCE_ACCURACY_VALUE',
'Maximum model space distance between geometric entities at asserted c
onnectivities');
#11716=UNCERTAINTY_MEASURE_WITH_UNIT(LENGTH_MEASURE(0.001),#11765,
'DISTANCE_ACCURACY_VALUE',
'Maximum model space distance between geometric entities at asserted c
onnectivities');
#11717=UNCERTAINTY_MEASURE_WITH_UNIT(LENGTH_MEASURE(0.001),#11765,
'DISTANCE_ACCURACY_VALUE',
'Maximum model space distance between geometric entities at asserted c
onnectivities');
#11718=UNCERTAINTY_MEASURE_WITH_UNIT(LENGTH_MEASURE(0.001),#11765,
'DISTANCE_ACCURACY_VALUE',
'Maximum model space distance between geometric entities at asserted c
onnectivities');
#11719=UNCERTAINTY_MEASURE_WITH_UNIT(LENGTH_MEASURE(0.001),#11765,
'DISTANCE_ACCURACY_VALUE',
'Maximum model space distance between geometric entities at asserted c
onnectivities');
#11720=UNCERTAINTY_MEASURE_WITH_UNIT(LENGTH_MEASURE(0.001),#11765,
'DISTANCE_ACCURACY_VALUE',
'Maximum model space distance between geometric entities at asserted c
onnectivities');
#11721=UNCERTAINTY_MEASURE_WITH_UNIT(LENGTH_MEASURE(0.001),#11765,
'DISTANCE_ACCURACY_VALUE',
'Maximum model space distance between geometric entities at asserted c
onnectivities');
#11722=UNCERTAINTY_MEASURE_WITH_UNIT(LENGTH_MEASURE(0.001),#11765,
'DISTANCE_ACCURACY_VALUE',
'Maximum model space distance between geometric entities at asserted c
onnectivities');
#11723=UNCERTAINTY_MEASURE_WITH_UNIT(LENGTH_MEASURE(0.001),#11765,
'DISTANCE_ACCURACY_VALUE',
'Maximum model space distance between geometric entities at asserted c
onnectivities');
#11724=UNCERTAINTY_MEASURE_WITH_UNIT(LENGTH_MEASURE(0.001),#11765,
'DISTANCE_ACCURACY_VALUE',
'Maximum model space distance between geometric entities at asserted c
onnectivities');
#11725=UNCERTAINTY_MEASURE_WITH_UNIT(LENGTH_MEASURE(0.001),#11765,
'DISTANCE_ACCURACY_VALUE',
'Maximum model space distance between geometric entities at asserted c
onnectivities');
#11726=UNCERTAINTY_MEASURE_WITH_UNIT(LENGTH_MEASURE(0.001),#11765,
'DISTANCE_ACCURACY_VALUE',
'Maximum model space distance between geometric entities at asserted c
onnectivities');
#11727=UNCERTAINTY_MEASURE_WITH_UNIT(LENGTH_MEASURE(0.001),#11765,
'DISTANCE_ACCURACY_VALUE',
'Maximum model space distance between geometric entities at asserted c
onnectivities');
#11728=UNCERTAINTY_MEASURE_WITH_UNIT(LENGTH_MEASURE(0.001),#11765,
'DISTANCE_ACCURACY_VALUE',
'Maximum model space distance between geometric entities at asserted c
onnectivities');
#11729=UNCERTAINTY_MEASURE_WITH_UNIT(LENGTH_MEASURE(0.001),#11765,
'DISTANCE_ACCURACY_VALUE',
'Maximum model space distance between geometric entities at asserted c
onnectivities');
#11730=UNCERTAINTY_MEASURE_WITH_UNIT(LENGTH_MEASURE(0.001),#11765,
'DISTANCE_ACCURACY_VALUE',
'Maximum model space distance between geometric entities at asserted c
onnectivities');
#11731=UNCERTAINTY_MEASURE_WITH_UNIT(LENGTH_MEASURE(0.001),#11765,
'DISTANCE_ACCURACY_VALUE',
'Maximum model space distance between geometric entities at asserted c
onnectivities');
#11732=UNCERTAINTY_MEASURE_WITH_UNIT(LENGTH_MEASURE(0.001),#11765,
'DISTANCE_ACCURACY_VALUE',
'Maximum model space distance between geometric entities at asserted c
onnectivities');
#11733=(
GEOMETRIC_REPRESENTATION_CONTEXT(3)
GLOBAL_UNCERTAINTY_ASSIGNED_CONTEXT((#11701))
GLOBAL_UNIT_ASSIGNED_CONTEXT((#11765,#11767,#11768))
REPRESENTATION_CONTEXT('','3D')
);
#11734=(
GEOMETRIC_REPRESENTATION_CONTEXT(3)
GLOBAL_UNCERTAINTY_ASSIGNED_CONTEXT((#11702))
GLOBAL_UNIT_ASSIGNED_CONTEXT((#11765,#11767,#11768))
REPRESENTATION_CONTEXT('','3D')
);
#11735=(
GEOMETRIC_REPRESENTATION_CONTEXT(3)
GLOBAL_UNCERTAINTY_ASSIGNED_CONTEXT((#11703))
GLOBAL_UNIT_ASSIGNED_CONTEXT((#11765,#11767,#11768))
REPRESENTATION_CONTEXT('','3D')
);
#11736=(
GEOMETRIC_REPRESENTATION_CONTEXT(3)
GLOBAL_UNCERTAINTY_ASSIGNED_CONTEXT((#11704))
GLOBAL_UNIT_ASSIGNED_CONTEXT((#11765,#11767,#11768))
REPRESENTATION_CONTEXT('','3D')
);
#11737=(
GEOMETRIC_REPRESENTATION_CONTEXT(3)
GLOBAL_UNCERTAINTY_ASSIGNED_CONTEXT((#11705))
GLOBAL_UNIT_ASSIGNED_CONTEXT((#11765,#11767,#11768))
REPRESENTATION_CONTEXT('','3D')
);
#11738=(
GEOMETRIC_REPRESENTATION_CONTEXT(3)
GLOBAL_UNCERTAINTY_ASSIGNED_CONTEXT((#11706))
GLOBAL_UNIT_ASSIGNED_CONTEXT((#11765,#11767,#11768))
REPRESENTATION_CONTEXT('','3D')
);
#11739=(
GEOMETRIC_REPRESENTATION_CONTEXT(3)
GLOBAL_UNCERTAINTY_ASSIGNED_CONTEXT((#11707))
GLOBAL_UNIT_ASSIGNED_CONTEXT((#11765,#11767,#11768))
REPRESENTATION_CONTEXT('','3D')
);
#11740=(
GEOMETRIC_REPRESENTATION_CONTEXT(3)
GLOBAL_UNCERTAINTY_ASSIGNED_CONTEXT((#11708))
GLOBAL_UNIT_ASSIGNED_CONTEXT((#11765,#11767,#11768))
REPRESENTATION_CONTEXT('','3D')
);
#11741=(
GEOMETRIC_REPRESENTATION_CONTEXT(3)
GLOBAL_UNCERTAINTY_ASSIGNED_CONTEXT((#11709))
GLOBAL_UNIT_ASSIGNED_CONTEXT((#11765,#11767,#11768))
REPRESENTATION_CONTEXT('','3D')
);
#11742=(
GEOMETRIC_REPRESENTATION_CONTEXT(3)
GLOBAL_UNCERTAINTY_ASSIGNED_CONTEXT((#11710))
GLOBAL_UNIT_ASSIGNED_CONTEXT((#11765,#11767,#11768))
REPRESENTATION_CONTEXT('','3D')
);
#11743=(
GEOMETRIC_REPRESENTATION_CONTEXT(3)
GLOBAL_UNCERTAINTY_ASSIGNED_CONTEXT((#11711))
GLOBAL_UNIT_ASSIGNED_CONTEXT((#11765,#11767,#11768))
REPRESENTATION_CONTEXT('','3D')
);
#11744=(
GEOMETRIC_REPRESENTATION_CONTEXT(3)
GLOBAL_UNCERTAINTY_ASSIGNED_CONTEXT((#11712))
GLOBAL_UNIT_ASSIGNED_CONTEXT((#11765,#11767,#11768))
REPRESENTATION_CONTEXT('','3D')
);
#11745=(
GEOMETRIC_REPRESENTATION_CONTEXT(3)
GLOBAL_UNCERTAINTY_ASSIGNED_CONTEXT((#11713))
GLOBAL_UNIT_ASSIGNED_CONTEXT((#11765,#11767,#11768))
REPRESENTATION_CONTEXT('','3D')
);
#11746=(
GEOMETRIC_REPRESENTATION_CONTEXT(3)
GLOBAL_UNCERTAINTY_ASSIGNED_CONTEXT((#11714))
GLOBAL_UNIT_ASSIGNED_CONTEXT((#11765,#11767,#11768))
REPRESENTATION_CONTEXT('','3D')
);
#11747=(
GEOMETRIC_REPRESENTATION_CONTEXT(3)
GLOBAL_UNCERTAINTY_ASSIGNED_CONTEXT((#11715))
GLOBAL_UNIT_ASSIGNED_CONTEXT((#11765,#11767,#11768))
REPRESENTATION_CONTEXT('','3D')
);
#11748=(
GEOMETRIC_REPRESENTATION_CONTEXT(3)
GLOBAL_UNCERTAINTY_ASSIGNED_CONTEXT((#11716))
GLOBAL_UNIT_ASSIGNED_CONTEXT((#11765,#11767,#11768))
REPRESENTATION_CONTEXT('','3D')
);
#11749=(
GEOMETRIC_REPRESENTATION_CONTEXT(3)
GLOBAL_UNCERTAINTY_ASSIGNED_CONTEXT((#11717))
GLOBAL_UNIT_ASSIGNED_CONTEXT((#11765,#11767,#11768))
REPRESENTATION_CONTEXT('','3D')
);
#11750=(
GEOMETRIC_REPRESENTATION_CONTEXT(3)
GLOBAL_UNCERTAINTY_ASSIGNED_CONTEXT((#11718))
GLOBAL_UNIT_ASSIGNED_CONTEXT((#11765,#11767,#11768))
REPRESENTATION_CONTEXT('','3D')
);
#11751=(
GEOMETRIC_REPRESENTATION_CONTEXT(3)
GLOBAL_UNCERTAINTY_ASSIGNED_CONTEXT((#11719))
GLOBAL_UNIT_ASSIGNED_CONTEXT((#11765,#11767,#11768))
REPRESENTATION_CONTEXT('','3D')
);
#11752=(
GEOMETRIC_REPRESENTATION_CONTEXT(3)
GLOBAL_UNCERTAINTY_ASSIGNED_CONTEXT((#11720))
GLOBAL_UNIT_ASSIGNED_CONTEXT((#11765,#11767,#11768))
REPRESENTATION_CONTEXT('','3D')
);
#11753=(
GEOMETRIC_REPRESENTATION_CONTEXT(3)
GLOBAL_UNCERTAINTY_ASSIGNED_CONTEXT((#11721))
GLOBAL_UNIT_ASSIGNED_CONTEXT((#11765,#11767,#11768))
REPRESENTATION_CONTEXT('','3D')
);
#11754=(
GEOMETRIC_REPRESENTATION_CONTEXT(3)
GLOBAL_UNCERTAINTY_ASSIGNED_CONTEXT((#11722))
GLOBAL_UNIT_ASSIGNED_CONTEXT((#11765,#11767,#11768))
REPRESENTATION_CONTEXT('','3D')
);
#11755=(
GEOMETRIC_REPRESENTATION_CONTEXT(3)
GLOBAL_UNCERTAINTY_ASSIGNED_CONTEXT((#11723))
GLOBAL_UNIT_ASSIGNED_CONTEXT((#11765,#11767,#11768))
REPRESENTATION_CONTEXT('','3D')
);
#11756=(
GEOMETRIC_REPRESENTATION_CONTEXT(3)
GLOBAL_UNCERTAINTY_ASSIGNED_CONTEXT((#11724))
GLOBAL_UNIT_ASSIGNED_CONTEXT((#11765,#11767,#11768))
REPRESENTATION_CONTEXT('','3D')
);
#11757=(
GEOMETRIC_REPRESENTATION_CONTEXT(3)
GLOBAL_UNCERTAINTY_ASSIGNED_CONTEXT((#11725))
GLOBAL_UNIT_ASSIGNED_CONTEXT((#11765,#11767,#11768))
REPRESENTATION_CONTEXT('','3D')
);
#11758=(
GEOMETRIC_REPRESENTATION_CONTEXT(3)
GLOBAL_UNCERTAINTY_ASSIGNED_CONTEXT((#11726))
GLOBAL_UNIT_ASSIGNED_CONTEXT((#11765,#11767,#11768))
REPRESENTATION_CONTEXT('','3D')
);
#11759=(
GEOMETRIC_REPRESENTATION_CONTEXT(3)
GLOBAL_UNCERTAINTY_ASSIGNED_CONTEXT((#11727))
GLOBAL_UNIT_ASSIGNED_CONTEXT((#11765,#11767,#11768))
REPRESENTATION_CONTEXT('','3D')
);
#11760=(
GEOMETRIC_REPRESENTATION_CONTEXT(3)
GLOBAL_UNCERTAINTY_ASSIGNED_CONTEXT((#11728))
GLOBAL_UNIT_ASSIGNED_CONTEXT((#11765,#11767,#11768))
REPRESENTATION_CONTEXT('','3D')
);
#11761=(
GEOMETRIC_REPRESENTATION_CONTEXT(3)
GLOBAL_UNCERTAINTY_ASSIGNED_CONTEXT((#11729))
GLOBAL_UNIT_ASSIGNED_CONTEXT((#11765,#11767,#11768))
REPRESENTATION_CONTEXT('','3D')
);
#11762=(
GEOMETRIC_REPRESENTATION_CONTEXT(3)
GLOBAL_UNCERTAINTY_ASSIGNED_CONTEXT((#11730))
GLOBAL_UNIT_ASSIGNED_CONTEXT((#11765,#11767,#11768))
REPRESENTATION_CONTEXT('','3D')
);
#11763=(
GEOMETRIC_REPRESENTATION_CONTEXT(3)
GLOBAL_UNCERTAINTY_ASSIGNED_CONTEXT((#11731))
GLOBAL_UNIT_ASSIGNED_CONTEXT((#11765,#11767,#11768))
REPRESENTATION_CONTEXT('','3D')
);
#11764=(
GEOMETRIC_REPRESENTATION_CONTEXT(3)
GLOBAL_UNCERTAINTY_ASSIGNED_CONTEXT((#11732))
GLOBAL_UNIT_ASSIGNED_CONTEXT((#11765,#11767,#11768))
REPRESENTATION_CONTEXT('','3D')
);
#11765=(
LENGTH_UNIT()
NAMED_UNIT(*)
SI_UNIT(.CENTI.,.METRE.)
);
#11766=(
LENGTH_UNIT()
NAMED_UNIT(*)
SI_UNIT($,.METRE.)
);
#11767=(
NAMED_UNIT(*)
PLANE_ANGLE_UNIT()
SI_UNIT($,.RADIAN.)
);
#11768=(
NAMED_UNIT(*)
SI_UNIT($,.STERADIAN.)
SOLID_ANGLE_UNIT()
);
#11769=SHAPE_DEFINITION_REPRESENTATION(#11800,#11878);
#11770=SHAPE_DEFINITION_REPRESENTATION(#11801,#11879);
#11771=SHAPE_DEFINITION_REPRESENTATION(#11802,#11880);
#11772=SHAPE_DEFINITION_REPRESENTATION(#11803,#11881);
#11773=SHAPE_DEFINITION_REPRESENTATION(#11804,#11882);
#11774=SHAPE_DEFINITION_REPRESENTATION(#11805,#11883);
#11775=SHAPE_DEFINITION_REPRESENTATION(#11806,#11884);
#11776=SHAPE_DEFINITION_REPRESENTATION(#11807,#11885);
#11777=SHAPE_DEFINITION_REPRESENTATION(#11808,#11886);
#11778=SHAPE_DEFINITION_REPRESENTATION(#11809,#11887);
#11779=SHAPE_DEFINITION_REPRESENTATION(#11810,#11888);
#11780=SHAPE_DEFINITION_REPRESENTATION(#11811,#11889);
#11781=SHAPE_DEFINITION_REPRESENTATION(#11812,#11890);
#11782=SHAPE_DEFINITION_REPRESENTATION(#11813,#11891);
#11783=SHAPE_DEFINITION_REPRESENTATION(#11816,#11892);
#11784=SHAPE_DEFINITION_REPRESENTATION(#11817,#11893);
#11785=SHAPE_DEFINITION_REPRESENTATION(#11818,#11894);
#11786=SHAPE_DEFINITION_REPRESENTATION(#11819,#11895);
#11787=SHAPE_DEFINITION_REPRESENTATION(#11820,#11896);
#11788=SHAPE_DEFINITION_REPRESENTATION(#11821,#11897);
#11789=SHAPE_DEFINITION_REPRESENTATION(#11822,#11898);
#11790=SHAPE_DEFINITION_REPRESENTATION(#11823,#11899);
#11791=SHAPE_DEFINITION_REPRESENTATION(#11824,#11900);
#11792=SHAPE_DEFINITION_REPRESENTATION(#11825,#11901);
#11793=SHAPE_DEFINITION_REPRESENTATION(#11826,#11902);
#11794=SHAPE_DEFINITION_REPRESENTATION(#11827,#11903);
#11795=SHAPE_DEFINITION_REPRESENTATION(#11828,#11904);
#11796=SHAPE_DEFINITION_REPRESENTATION(#11829,#11905);
#11797=SHAPE_DEFINITION_REPRESENTATION(#11830,#11906);
#11798=SHAPE_DEFINITION_REPRESENTATION(#11831,#11907);
#11799=SHAPE_DEFINITION_REPRESENTATION(#11832,#11908);
#11800=PRODUCT_DEFINITION_SHAPE('',$,#11910);
#11801=PRODUCT_DEFINITION_SHAPE('',$,#11911);
#11802=PRODUCT_DEFINITION_SHAPE('',$,#11912);
#11803=PRODUCT_DEFINITION_SHAPE('',$,#11913);
#11804=PRODUCT_DEFINITION_SHAPE('',$,#11914);
#11805=PRODUCT_DEFINITION_SHAPE('',$,#11915);
#11806=PRODUCT_DEFINITION_SHAPE('',$,#11916);
#11807=PRODUCT_DEFINITION_SHAPE('',$,#11917);
#11808=PRODUCT_DEFINITION_SHAPE('',$,#11918);
#11809=PRODUCT_DEFINITION_SHAPE('',$,#11919);
#11810=PRODUCT_DEFINITION_SHAPE('',$,#11920);
#11811=PRODUCT_DEFINITION_SHAPE('',$,#11921);
#11812=PRODUCT_DEFINITION_SHAPE('',$,#11922);
#11813=PRODUCT_DEFINITION_SHAPE('',$,#11923);
#11814=PRODUCT_DEFINITION_SHAPE($,$,#164);
#11815=PRODUCT_DEFINITION_SHAPE($,$,#165);
#11816=PRODUCT_DEFINITION_SHAPE('',$,#11924);
#11817=PRODUCT_DEFINITION_SHAPE('',$,#11925);
#11818=PRODUCT_DEFINITION_SHAPE('',$,#11926);
#11819=PRODUCT_DEFINITION_SHAPE('',$,#11927);
#11820=PRODUCT_DEFINITION_SHAPE('',$,#11928);
#11821=PRODUCT_DEFINITION_SHAPE('',$,#11929);
#11822=PRODUCT_DEFINITION_SHAPE('',$,#11930);
#11823=PRODUCT_DEFINITION_SHAPE('',$,#11931);
#11824=PRODUCT_DEFINITION_SHAPE('',$,#11932);
#11825=PRODUCT_DEFINITION_SHAPE('',$,#11933);
#11826=PRODUCT_DEFINITION_SHAPE('',$,#11934);
#11827=PRODUCT_DEFINITION_SHAPE('',$,#11935);
#11828=PRODUCT_DEFINITION_SHAPE('',$,#11936);
#11829=PRODUCT_DEFINITION_SHAPE('',$,#11937);
#11830=PRODUCT_DEFINITION_SHAPE('',$,#11938);
#11831=PRODUCT_DEFINITION_SHAPE('',$,#11939);
#11832=PRODUCT_DEFINITION_SHAPE('',$,#11940);
#11833=PRODUCT_DEFINITION_SHAPE($,$,#166);
#11834=PRODUCT_DEFINITION_SHAPE($,$,#167);
#11835=PRODUCT_DEFINITION_SHAPE($,$,#168);
#11836=PRODUCT_DEFINITION_SHAPE($,$,#169);
#11837=PRODUCT_DEFINITION_SHAPE($,$,#170);
#11838=PRODUCT_DEFINITION_SHAPE($,$,#171);
#11839=PRODUCT_DEFINITION_SHAPE($,$,#172);
#11840=PRODUCT_DEFINITION_SHAPE($,$,#173);
#11841=PRODUCT_DEFINITION_SHAPE($,$,#174);
#11842=PRODUCT_DEFINITION_SHAPE($,$,#175);
#11843=PRODUCT_DEFINITION_SHAPE($,$,#176);
#11844=PRODUCT_DEFINITION_SHAPE($,$,#177);
#11845=PRODUCT_DEFINITION_SHAPE($,$,#178);
#11846=PRODUCT_DEFINITION_SHAPE($,$,#179);
#11847=PRODUCT_DEFINITION_SHAPE($,$,#180);
#11848=PRODUCT_DEFINITION_SHAPE($,$,#181);
#11849=PRODUCT_DEFINITION_SHAPE($,$,#182);
#11850=PRODUCT_DEFINITION_SHAPE($,$,#183);
#11851=PRODUCT_DEFINITION_SHAPE($,$,#184);
#11852=PRODUCT_DEFINITION_SHAPE($,$,#185);
#11853=PRODUCT_DEFINITION_SHAPE($,$,#186);
#11854=PRODUCT_DEFINITION_SHAPE($,$,#187);
#11855=PRODUCT_DEFINITION_SHAPE($,$,#188);
#11856=PRODUCT_DEFINITION_SHAPE($,$,#189);
#11857=PRODUCT_DEFINITION_SHAPE($,$,#190);
#11858=PRODUCT_DEFINITION_SHAPE($,$,#191);
#11859=PRODUCT_DEFINITION_SHAPE($,$,#192);
#11860=PRODUCT_DEFINITION_SHAPE($,$,#193);
#11861=PRODUCT_DEFINITION_SHAPE($,$,#194);
#11862=PRODUCT_DEFINITION_SHAPE($,$,#195);
#11863=PRODUCT_DEFINITION_SHAPE($,$,#196);
#11864=PRODUCT_DEFINITION_SHAPE($,$,#197);
#11865=PRODUCT_DEFINITION_SHAPE($,$,#198);
#11866=PRODUCT_DEFINITION_SHAPE($,$,#199);
#11867=PRODUCT_DEFINITION_SHAPE($,$,#200);
#11868=PRODUCT_DEFINITION_SHAPE($,$,#201);
#11869=PRODUCT_DEFINITION_SHAPE($,$,#202);
#11870=PRODUCT_DEFINITION_SHAPE($,$,#203);
#11871=PRODUCT_DEFINITION_SHAPE($,$,#204);
#11872=PRODUCT_DEFINITION_SHAPE($,$,#205);
#11873=PRODUCT_DEFINITION_SHAPE($,$,#206);
#11874=PRODUCT_DEFINITION_SHAPE($,$,#207);
#11875=PRODUCT_DEFINITION_SHAPE($,$,#208);
#11876=PRODUCT_DEFINITION_SHAPE($,$,#209);
#11877=PRODUCT_DEFINITION_SHAPE($,$,#210);
#11878=SHAPE_REPRESENTATION('',(#6459,#7206,#7207),#11733);
#11879=SHAPE_REPRESENTATION('',(#6460,#7163,#7164,#7165,#7166,#7167,#7168,
#7169,#7170,#7171,#7172,#7173,#7174,#7175,#7176,#7177,#7178,#7179,#7180,
#7181,#7182,#7183,#7184,#7185,#7186,#7187,#7188,#7189),#11734);
#11880=SHAPE_REPRESENTATION('',(#6461),#11735);
#11881=SHAPE_REPRESENTATION('',(#6474),#11736);
#11882=SHAPE_REPRESENTATION('',(#6504),#11737);
#11883=SHAPE_REPRESENTATION('',(#6513),#11738);
#11884=SHAPE_REPRESENTATION('',(#6522),#11739);
#11885=SHAPE_REPRESENTATION('',(#6531),#11740);
#11886=SHAPE_REPRESENTATION('',(#6540),#11741);
#11887=SHAPE_REPRESENTATION('',(#6547),#11742);
#11888=SHAPE_REPRESENTATION('',(#6554),#11743);
#11889=SHAPE_REPRESENTATION('',(#6578,#6646,#6647),#11744);
#11890=SHAPE_REPRESENTATION('',(#6579),#11745);
#11891=SHAPE_REPRESENTATION('',(#6618),#11746);
#11892=SHAPE_REPRESENTATION('',(#6648),#11747);
#11893=SHAPE_REPRESENTATION('',(#6674,#7190,#7191,#7192,#7193,#7194,#7195,
#7196,#7197,#7198,#7199,#7200,#7201,#7202,#7203,#7204,#7205),#11748);
#11894=SHAPE_REPRESENTATION('',(#6675),#11749);
#11895=SHAPE_REPRESENTATION('',(#6707),#11750);
#11896=SHAPE_REPRESENTATION('',(#6716),#11751);
#11897=SHAPE_REPRESENTATION('',(#6725),#11752);
#11898=SHAPE_REPRESENTATION('',(#6734),#11753);
#11899=SHAPE_REPRESENTATION('',(#6749),#11754);
#11900=SHAPE_REPRESENTATION('',(#6764),#11755);
#11901=SHAPE_REPRESENTATION('',(#6798),#11756);
#11902=SHAPE_REPRESENTATION('',(#6807),#11757);
#11903=SHAPE_REPRESENTATION('',(#7073),#11758);
#11904=SHAPE_REPRESENTATION('',(#7084),#11759);
#11905=SHAPE_REPRESENTATION('',(#7110),#11760);
#11906=SHAPE_REPRESENTATION('',(#7127),#11761);
#11907=SHAPE_REPRESENTATION('',(#7138),#11762);
#11908=SHAPE_REPRESENTATION('',(#7147),#11763);
#11909=PRODUCT_DEFINITION_CONTEXT('part definition',#12004,'design');
#11910=PRODUCT_DEFINITION('PAT-036','PAT-036',#11941,#11909);
#11911=PRODUCT_DEFINITION('Flange bearing stand','Flange bearing stand',
#11942,#11909);
#11912=PRODUCT_DEFINITION('Base','Base',#11943,#11909);
#11913=PRODUCT_DEFINITION('Bearing wall','Bearing wall',#11944,#11909);
#11914=PRODUCT_DEFINITION('Flange hole reducer','Flange hole reducer',#11945,
#11909);
#11915=PRODUCT_DEFINITION('Flange hole reducer (1)',
'Flange hole reducer (1)',#11946,#11909);
#11916=PRODUCT_DEFINITION('Flange hole reducer (2)',
'Flange hole reducer (2)',#11947,#11909);
#11917=PRODUCT_DEFINITION('Flange hole reducer (3)',
'Flange hole reducer (3)',#11948,#11909);
#11918=PRODUCT_DEFINITION('Bonded foot pad','Bonded foot pad',#11949,#11909);
#11919=PRODUCT_DEFINITION('Bonded foot pad (1)','Bonded foot pad (1)',#11950,
#11909);
#11920=PRODUCT_DEFINITION('M6x18 mounting screw','M6x18 mounting screw',
#11951,#11909);
#11921=PRODUCT_DEFINITION('Square Flange Bearing - 20 mm Bore',
'Square Flange Bearing - 20 mm Bore',#11952,#11909);
#11922=PRODUCT_DEFINITION('Housing','Housing',#11953,#11909);
#11923=PRODUCT_DEFINITION('Insert bearing','Insert bearing',#11954,#11909);
#11924=PRODUCT_DEFINITION('Cap Screw - M8x30','Cap Screw - M8x30',#11955,
#11909);
#11925=PRODUCT_DEFINITION('Stepped spindle (1)','Stepped spindle (1)',#11956,
#11909);
#11926=PRODUCT_DEFINITION('Stepped spindle','Stepped spindle',#11957,
#11909);
#11927=PRODUCT_DEFINITION('Pulley inner spacer','Pulley inner spacer',#11958,
#11909);
#11928=PRODUCT_DEFINITION('Pulley outer spacer','Pulley outer spacer',#11959,
#11909);
#11929=PRODUCT_DEFINITION('Pulley keeper','Pulley keeper',#11960,#11909);
#11930=PRODUCT_DEFINITION('Shaft collar','Shaft collar',#11961,#11909);
#11931=PRODUCT_DEFINITION('Shaft collar (1)','Shaft collar (1)',#11962,#11909);
#11932=PRODUCT_DEFINITION('Faceplate','Faceplate',#11963,#11909);
#11933=PRODUCT_DEFINITION('Drawbar keeper','Drawbar keeper',#11964,#11909);
#11934=PRODUCT_DEFINITION(
'Timing Pulley - 2 mm Pitch, 40 Teeth, 12 mm Bore',
'Timing Pulley - 2 mm Pitch, 40 Teeth, 12 mm Bore',#11965,#11909);
#11935=PRODUCT_DEFINITION('Key 4x4x14','Key 4x4x14',#11966,#11909);
#11936=PRODUCT_DEFINITION('Cap Screw - M5x20','Cap Screw - M5x20',#11967,
#11909);
#11937=PRODUCT_DEFINITION('Socket Set Screw - M5x8',
'Socket Set Screw - M5x8',#11968,#11909);
#11938=PRODUCT_DEFINITION('Key 6x6x20','Key 6x6x20',#11969,#11909);
#11939=PRODUCT_DEFINITION('Flat Washer - M8','Flat Washer - M8',#11970,
#11909);
#11940=PRODUCT_DEFINITION('Hex Nut - M8','Hex Nut - M8',#11971,#11909);
#11941=PRODUCT_DEFINITION_FORMATION('',$,#12006);
#11942=PRODUCT_DEFINITION_FORMATION('',$,#12007);
#11943=PRODUCT_DEFINITION_FORMATION('',$,#12008);
#11944=PRODUCT_DEFINITION_FORMATION('',$,#12009);
#11945=PRODUCT_DEFINITION_FORMATION('',$,#12010);
#11946=PRODUCT_DEFINITION_FORMATION('',$,#12011);
#11947=PRODUCT_DEFINITION_FORMATION('',$,#12012);
#11948=PRODUCT_DEFINITION_FORMATION('',$,#12013);
#11949=PRODUCT_DEFINITION_FORMATION('',$,#12014);
#11950=PRODUCT_DEFINITION_FORMATION('',$,#12015);
#11951=PRODUCT_DEFINITION_FORMATION('',$,#12016);
#11952=PRODUCT_DEFINITION_FORMATION('',$,#12017);
#11953=PRODUCT_DEFINITION_FORMATION('',$,#12018);
#11954=PRODUCT_DEFINITION_FORMATION('',$,#12019);
#11955=PRODUCT_DEFINITION_FORMATION('',$,#12020);
#11956=PRODUCT_DEFINITION_FORMATION('',$,#12021);
#11957=PRODUCT_DEFINITION_FORMATION('',$,#12022);
#11958=PRODUCT_DEFINITION_FORMATION('',$,#12023);
#11959=PRODUCT_DEFINITION_FORMATION('',$,#12024);
#11960=PRODUCT_DEFINITION_FORMATION('',$,#12025);
#11961=PRODUCT_DEFINITION_FORMATION('',$,#12026);
#11962=PRODUCT_DEFINITION_FORMATION('',$,#12027);
#11963=PRODUCT_DEFINITION_FORMATION('',$,#12028);
#11964=PRODUCT_DEFINITION_FORMATION('',$,#12029);
#11965=PRODUCT_DEFINITION_FORMATION('',$,#12030);
#11966=PRODUCT_DEFINITION_FORMATION('',$,#12031);
#11967=PRODUCT_DEFINITION_FORMATION('',$,#12032);
#11968=PRODUCT_DEFINITION_FORMATION('',$,#12033);
#11969=PRODUCT_DEFINITION_FORMATION('',$,#12034);
#11970=PRODUCT_DEFINITION_FORMATION('',$,#12035);
#11971=PRODUCT_DEFINITION_FORMATION('',$,#12036);
#11972=PRODUCT_RELATED_PRODUCT_CATEGORY('PAT-036','PAT-036',(#12006));
#11973=PRODUCT_RELATED_PRODUCT_CATEGORY('Flange bearing stand',
'Flange bearing stand',(#12007));
#11974=PRODUCT_RELATED_PRODUCT_CATEGORY('Base','Base',(#12008));
#11975=PRODUCT_RELATED_PRODUCT_CATEGORY('Bearing wall','Bearing wall',(#12009));
#11976=PRODUCT_RELATED_PRODUCT_CATEGORY('Flange hole reducer',
'Flange hole reducer',(#12010));
#11977=PRODUCT_RELATED_PRODUCT_CATEGORY('Flange hole reducer (1)',
'Flange hole reducer (1)',(#12011));
#11978=PRODUCT_RELATED_PRODUCT_CATEGORY('Flange hole reducer (2)',
'Flange hole reducer (2)',(#12012));
#11979=PRODUCT_RELATED_PRODUCT_CATEGORY('Flange hole reducer (3)',
'Flange hole reducer (3)',(#12013));
#11980=PRODUCT_RELATED_PRODUCT_CATEGORY('Bonded foot pad',
'Bonded foot pad',(#12014));
#11981=PRODUCT_RELATED_PRODUCT_CATEGORY('Bonded foot pad (1)',
'Bonded foot pad (1)',(#12015));
#11982=PRODUCT_RELATED_PRODUCT_CATEGORY('M6x18 mounting screw',
'M6x18 mounting screw',(#12016));
#11983=PRODUCT_RELATED_PRODUCT_CATEGORY(
'Square Flange Bearing - 20 mm Bore',
'Square Flange Bearing - 20 mm Bore',(#12017));
#11984=PRODUCT_RELATED_PRODUCT_CATEGORY('Housing','Housing',(#12018));
#11985=PRODUCT_RELATED_PRODUCT_CATEGORY('Insert bearing',
'Insert bearing',(#12019));
#11986=PRODUCT_RELATED_PRODUCT_CATEGORY('Cap Screw - M8x30',
'Cap Screw - M8x30',(#12020));
#11987=PRODUCT_RELATED_PRODUCT_CATEGORY('Stepped spindle (1)',
'Stepped spindle (1)',(#12021));
#11988=PRODUCT_RELATED_PRODUCT_CATEGORY('Stepped spindle',
'Stepped spindle',(#12022));
#11989=PRODUCT_RELATED_PRODUCT_CATEGORY('Pulley inner spacer',
'Pulley inner spacer',(#12023));
#11990=PRODUCT_RELATED_PRODUCT_CATEGORY('Pulley outer spacer',
'Pulley outer spacer',(#12024));
#11991=PRODUCT_RELATED_PRODUCT_CATEGORY('Pulley keeper','Pulley keeper',
(#12025));
#11992=PRODUCT_RELATED_PRODUCT_CATEGORY('Shaft collar','Shaft collar',(#12026));
#11993=PRODUCT_RELATED_PRODUCT_CATEGORY('Shaft collar (1)',
'Shaft collar (1)',(#12027));
#11994=PRODUCT_RELATED_PRODUCT_CATEGORY('Faceplate','Faceplate',(#12028));
#11995=PRODUCT_RELATED_PRODUCT_CATEGORY('Drawbar keeper',
'Drawbar keeper',(#12029));
#11996=PRODUCT_RELATED_PRODUCT_CATEGORY(
'Timing Pulley - 2 mm Pitch, 40 Teeth, 12 mm Bore',
'Timing Pulley - 2 mm Pitch, 40 Teeth, 12 mm Bore',(#12030));
#11997=PRODUCT_RELATED_PRODUCT_CATEGORY('Key 4x4x14','Key 4x4x14',(#12031));
#11998=PRODUCT_RELATED_PRODUCT_CATEGORY('Cap Screw - M5x20',
'Cap Screw - M5x20',(#12032));
#11999=PRODUCT_RELATED_PRODUCT_CATEGORY('Socket Set Screw - M5x8',
'Socket Set Screw - M5x8',(#12033));
#12000=PRODUCT_RELATED_PRODUCT_CATEGORY('Key 6x6x20','Key 6x6x20',(#12034));
#12001=PRODUCT_RELATED_PRODUCT_CATEGORY('Flat Washer - M8',
'Flat Washer - M8',(#12035));
#12002=PRODUCT_RELATED_PRODUCT_CATEGORY('Hex Nut - M8','Hex Nut - M8',(#12036));
#12003=APPLICATION_PROTOCOL_DEFINITION('international standard',
'automotive_design',2009,#12004);
#12004=APPLICATION_CONTEXT(
'Core Data for Automotive Mechanical Design Process');
#12005=PRODUCT_CONTEXT('part definition',#12004,'mechanical');
#12006=PRODUCT('PAT-036','PAT-036',
'PAT-036',(#12005));
#12007=PRODUCT('Flange bearing stand','Flange bearing stand',
'Flange bearing stand',(#12005));
#12008=PRODUCT('Base','Base','Base',(#12005));
#12009=PRODUCT('Bearing wall','Bearing wall','Bearing wall',(#12005));
#12010=PRODUCT('Flange hole reducer','Flange hole reducer',
'Flange hole reducer',(#12005));
#12011=PRODUCT('Flange hole reducer (1)','Flange hole reducer (1)',
'Flange hole reducer (1)',(#12005));
#12012=PRODUCT('Flange hole reducer (2)','Flange hole reducer (2)',
'Flange hole reducer (2)',(#12005));
#12013=PRODUCT('Flange hole reducer (3)','Flange hole reducer (3)',
'Flange hole reducer (3)',(#12005));
#12014=PRODUCT('Bonded foot pad','Bonded foot pad','Bonded foot pad',(#12005));
#12015=PRODUCT('Bonded foot pad (1)','Bonded foot pad (1)',
'Bonded foot pad (1)',(#12005));
#12016=PRODUCT('M6x18 mounting screw','M6x18 mounting screw',
'M6x18 mounting screw',(#12005));
#12017=PRODUCT('Square Flange Bearing - 20 mm Bore',
'Square Flange Bearing - 20 mm Bore',
'Square Flange Bearing - 20 mm Bore',(#12005));
#12018=PRODUCT('Housing','Housing','Housing',(#12005));
#12019=PRODUCT('Insert bearing','Insert bearing','Insert bearing',(#12005));
#12020=PRODUCT('Cap Screw - M8x30','Cap Screw - M8x30',
'Cap Screw - M8x30',(#12005));
#12021=PRODUCT('Stepped spindle (1)','Stepped spindle (1)',
'Stepped spindle (1)',(#12005));
#12022=PRODUCT('Stepped spindle','Stepped spindle','Stepped spindle',
(#12005));
#12023=PRODUCT('Pulley inner spacer','Pulley inner spacer',
'Pulley inner spacer',(#12005));
#12024=PRODUCT('Pulley outer spacer','Pulley outer spacer',
'Pulley outer spacer',(#12005));
#12025=PRODUCT('Pulley keeper','Pulley keeper','Pulley keeper',(#12005));
#12026=PRODUCT('Shaft collar','Shaft collar','Shaft collar',(#12005));
#12027=PRODUCT('Shaft collar (1)','Shaft collar (1)','Shaft collar (1)',(#12005));
#12028=PRODUCT('Faceplate','Faceplate','Faceplate',(#12005));
#12029=PRODUCT('Drawbar keeper','Drawbar keeper','Drawbar keeper',(#12005));
#12030=PRODUCT('Timing Pulley - 2 mm Pitch, 40 Teeth, 12 mm Bore',
'Timing Pulley - 2 mm Pitch, 40 Teeth, 12 mm Bore',
'Timing Pulley - 2 mm Pitch, 40 Teeth, 12 mm Bore',(#12005));
#12031=PRODUCT('Key 4x4x14','Key 4x4x14','Key 4x4x14',(#12005));
#12032=PRODUCT('Cap Screw - M5x20','Cap Screw - M5x20',
'Cap Screw - M5x20',(#12005));
#12033=PRODUCT('Socket Set Screw - M5x8','Socket Set Screw - M5x8',
'Socket Set Screw - M5x8',(#12005));
#12034=PRODUCT('Key 6x6x20','Key 6x6x20','Key 6x6x20',(#12005));
#12035=PRODUCT('Flat Washer - M8','Flat Washer - M8','Flat Washer - M8',
(#12005));
#12036=PRODUCT('Hex Nut - M8','Hex Nut - M8','Hex Nut - M8',(#12005));
#12037=PRESENTATION_STYLE_ASSIGNMENT((#12042));
#12038=PRESENTATION_STYLE_ASSIGNMENT((#12043));
#12039=PRESENTATION_STYLE_ASSIGNMENT((#12044));
#12040=PRESENTATION_STYLE_ASSIGNMENT((#12045));
#12041=PRESENTATION_STYLE_ASSIGNMENT((#12046));
#12042=SURFACE_STYLE_USAGE(.BOTH.,#12047);
#12043=SURFACE_STYLE_USAGE(.BOTH.,#12048);
#12044=SURFACE_STYLE_USAGE(.BOTH.,#12049);
#12045=SURFACE_STYLE_USAGE(.BOTH.,#12050);
#12046=SURFACE_STYLE_USAGE(.BOTH.,#12051);
#12047=SURFACE_SIDE_STYLE('',(#12052));
#12048=SURFACE_SIDE_STYLE('',(#12053));
#12049=SURFACE_SIDE_STYLE('',(#12054));
#12050=SURFACE_SIDE_STYLE('',(#12055));
#12051=SURFACE_SIDE_STYLE('',(#12056));
#12052=SURFACE_STYLE_FILL_AREA(#12057);
#12053=SURFACE_STYLE_FILL_AREA(#12058);
#12054=SURFACE_STYLE_FILL_AREA(#12059);
#12055=SURFACE_STYLE_FILL_AREA(#12060);
#12056=SURFACE_STYLE_FILL_AREA(#12061);
#12057=FILL_AREA_STYLE('Steel - Satin',(#12062));
#12058=FILL_AREA_STYLE('CAD Library Painted - Deep blue',(#12063));
#12059=FILL_AREA_STYLE('CAD Library Painted - Steel gray',(#12064));
#12060=FILL_AREA_STYLE('CAD Library Painted - Engineering blue',(#12065));
#12061=FILL_AREA_STYLE('CAD Library Painted - Graphite',(#12066));
#12062=FILL_AREA_STYLE_COLOUR('Steel - Satin',#12067);
#12063=FILL_AREA_STYLE_COLOUR('CAD Library Painted - Deep blue',#12068);
#12064=FILL_AREA_STYLE_COLOUR('CAD Library Painted - Steel gray',#12069);
#12065=FILL_AREA_STYLE_COLOUR('CAD Library Painted - Engineering blue',
#12070);
#12066=FILL_AREA_STYLE_COLOUR('CAD Library Painted - Graphite',#12071);
#12067=COLOUR_RGB('Steel - Satin',0.627450980392157,0.627450980392157,0.627450980392157);
#12068=COLOUR_RGB('CAD Library Painted - Deep blue',0.0784313725490196,
0.203921568627451,0.349019607843137);
#12069=COLOUR_RGB('CAD Library Painted - Steel gray',0.592156862745098,
0.631372549019608,0.67843137254902);
#12070=COLOUR_RGB('CAD Library Painted - Engineering blue',0.12156862745098,
0.356862745098039,0.6);
#12071=COLOUR_RGB('CAD Library Painted - Graphite',0.168627450980392,0.192156862745098,
0.231372549019608);
#12072=COLOUR_RGB('Dark Blue',0.08,0.2,0.34);
#12073=FILL_AREA_STYLE_COLOUR('',#12072);
#12074=FILL_AREA_STYLE('',(#12073));
#12075=SURFACE_STYLE_FILL_AREA(#12074);
#12076=SURFACE_SIDE_STYLE('',(#12075));
#12077=SURFACE_STYLE_USAGE(.BOTH.,#12076);
#12078=PRESENTATION_STYLE_ASSIGNMENT((#12077));
#12079=COLOUR_RGB('Light Blue',0.38,0.62,0.78);
#12080=FILL_AREA_STYLE_COLOUR('',#12079);
#12081=FILL_AREA_STYLE('',(#12080));
#12082=SURFACE_STYLE_FILL_AREA(#12081);
#12083=SURFACE_SIDE_STYLE('',(#12082));
#12084=SURFACE_STYLE_USAGE(.BOTH.,#12083);
#12085=PRESENTATION_STYLE_ASSIGNMENT((#12084));
#12086=COLOUR_RGB('Sky Blue',0.24,0.69,0.87);
#12087=FILL_AREA_STYLE_COLOUR('',#12086);
#12088=FILL_AREA_STYLE('',(#12087));
#12089=SURFACE_STYLE_FILL_AREA(#12088);
#12090=SURFACE_SIDE_STYLE('',(#12089));
#12091=SURFACE_STYLE_USAGE(.BOTH.,#12090);
#12092=PRESENTATION_STYLE_ASSIGNMENT((#12091));
#12093=COLOUR_RGB('Grey',0.48,0.52,0.57);
#12094=FILL_AREA_STYLE_COLOUR('',#12093);
#12095=FILL_AREA_STYLE('',(#12094));
#12096=SURFACE_STYLE_FILL_AREA(#12095);
#12097=SURFACE_SIDE_STYLE('',(#12096));
#12098=SURFACE_STYLE_USAGE(.BOTH.,#12097);
#12099=PRESENTATION_STYLE_ASSIGNMENT((#12098));
#12100=COLOUR_RGB('Black',0.12,0.14,0.17);
#12101=FILL_AREA_STYLE_COLOUR('',#12100);
#12102=FILL_AREA_STYLE('',(#12101));
#12103=SURFACE_STYLE_FILL_AREA(#12102);
#12104=SURFACE_SIDE_STYLE('',(#12103));
#12105=SURFACE_STYLE_USAGE(.BOTH.,#12104);
#12106=PRESENTATION_STYLE_ASSIGNMENT((#12105));
#12107=COLOUR_RGB('Off White',0.89,0.88,0.83);
#12108=FILL_AREA_STYLE_COLOUR('',#12107);
#12109=FILL_AREA_STYLE('',(#12108));
#12110=SURFACE_STYLE_FILL_AREA(#12109);
#12111=SURFACE_SIDE_STYLE('',(#12110));
#12112=SURFACE_STYLE_USAGE(.BOTH.,#12111);
#12113=PRESENTATION_STYLE_ASSIGNMENT((#12112));
ENDSEC;
END-ISO-10303-21;
